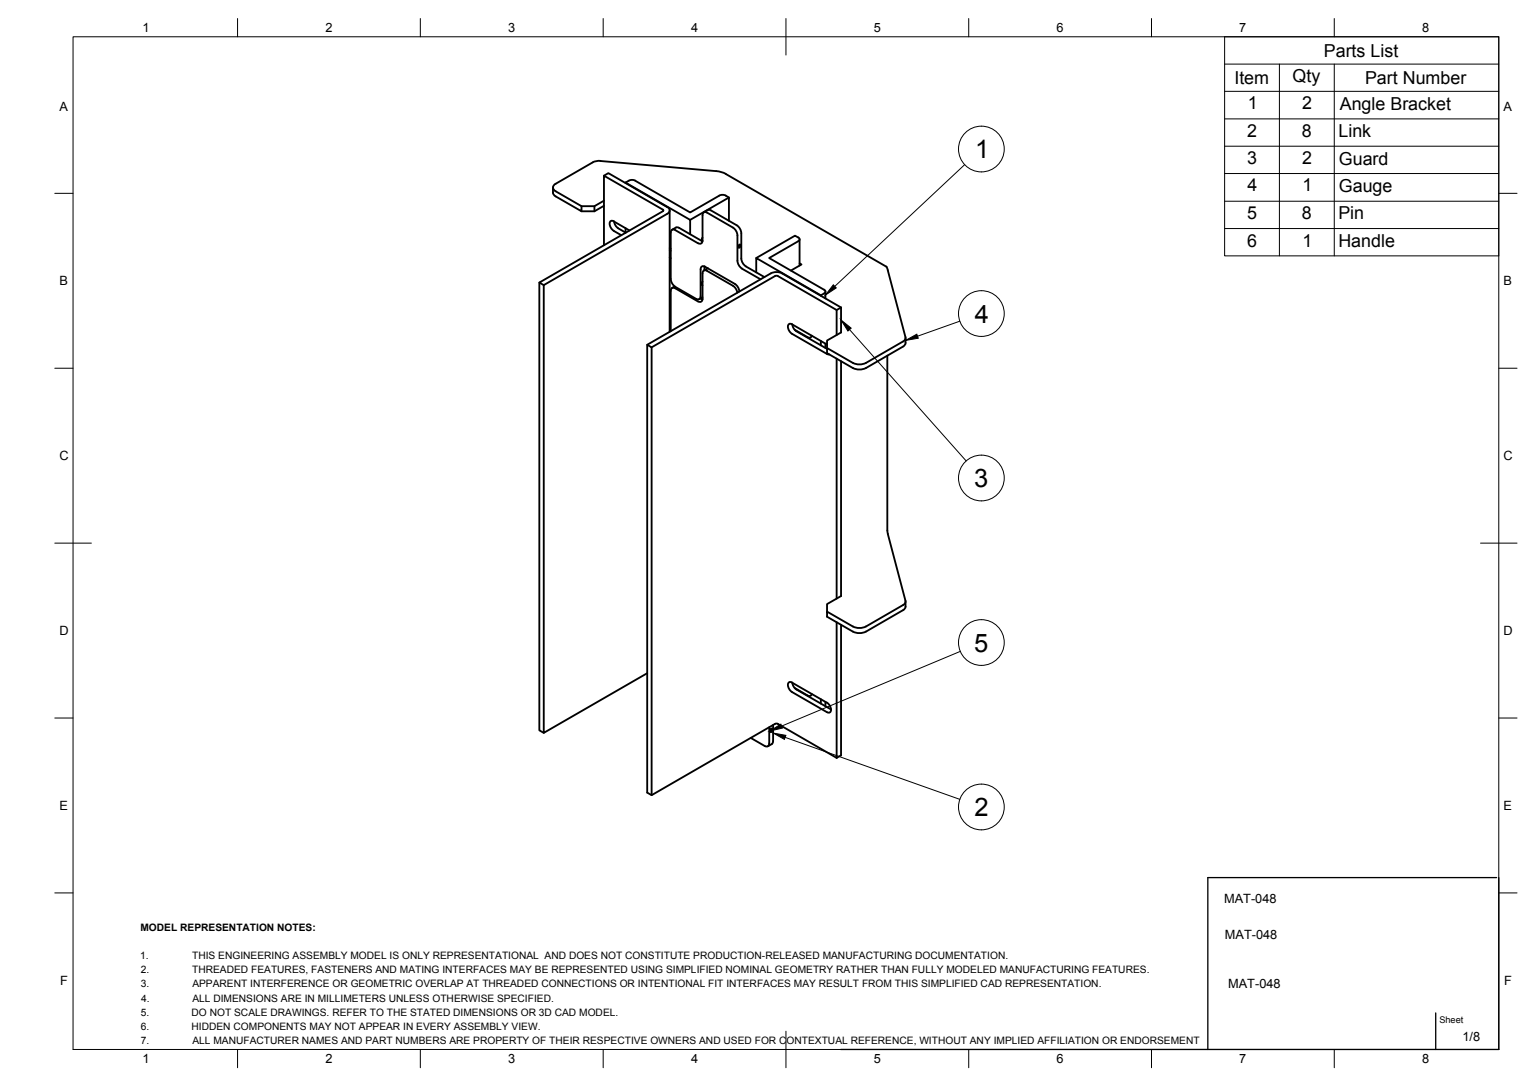
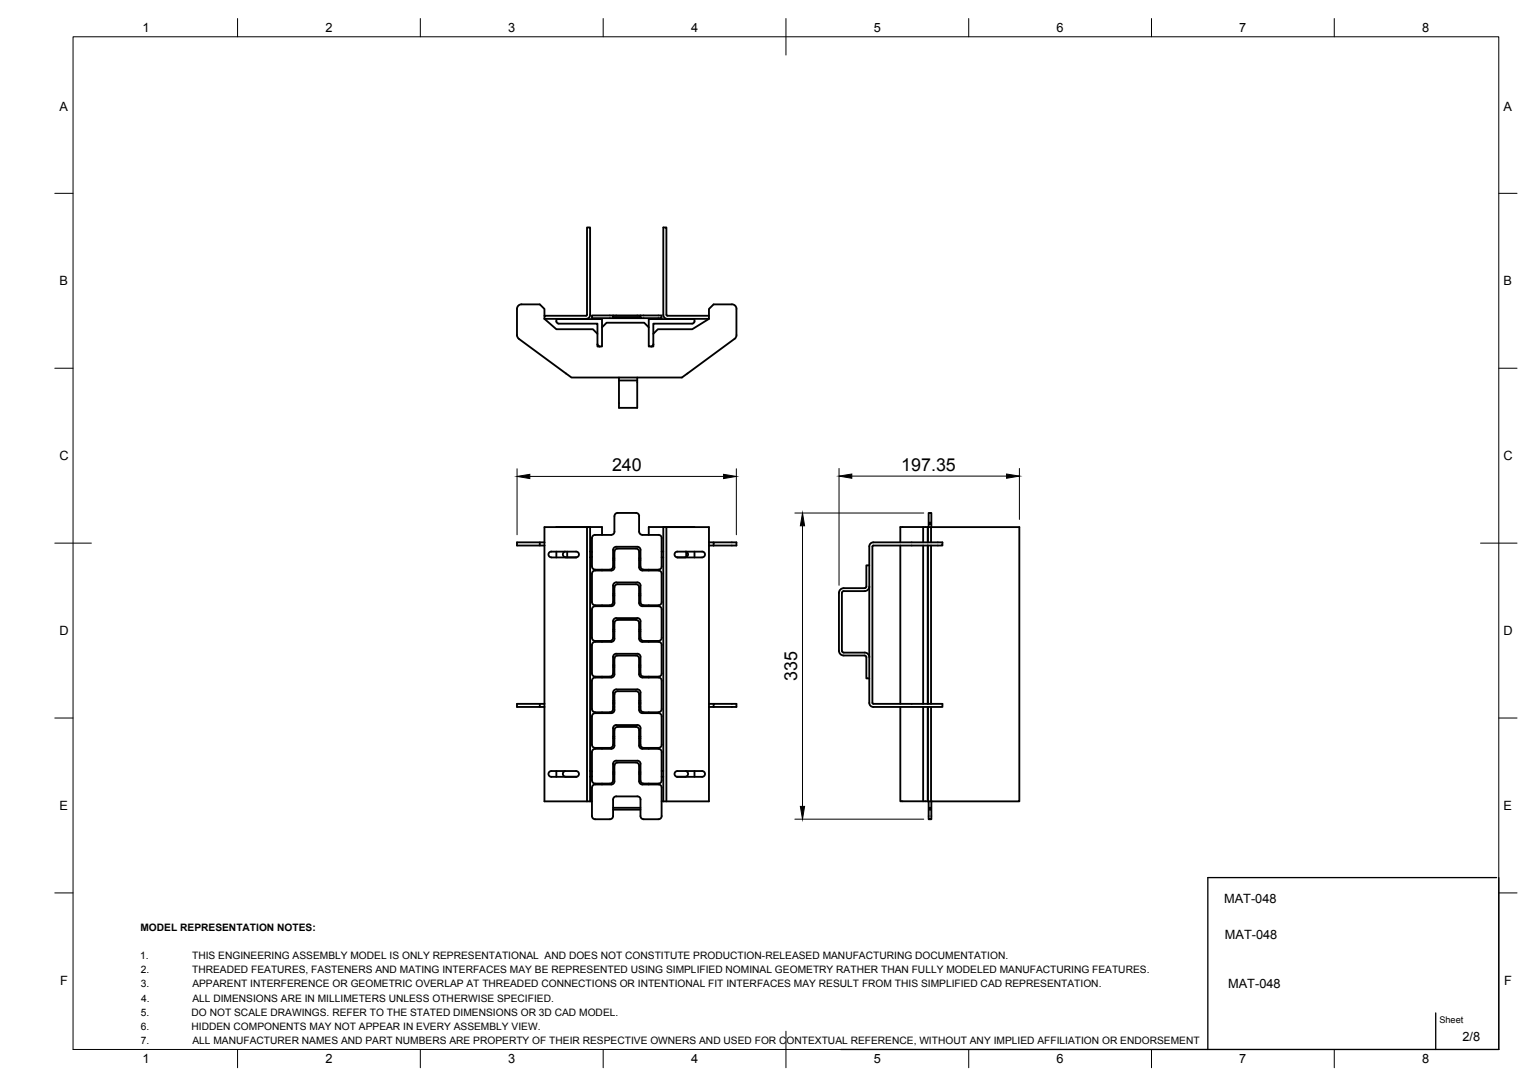
ISO-10303-21;
HEADER;
/* Generated by software containing ST-Developer
 * from STEP Tools, Inc. (www.steptools.com) 
 */

FILE_DESCRIPTION(
/* description */ ('STEP AP214'),
/* implementation_level */ '2;1');

FILE_NAME(
/* name */ 'MAT-048.step',
/* time_stamp */ '2026-11-14T22:24:45-08:00',
/* author */ (''),
/* organization */ (''),
/* preprocessor_version */ 'ST-DEVELOPER v20.2',
/* originating_system */ 'Autodesk Translation Framework v15.17.0.0',
/* authorisation */ '');

FILE_SCHEMA (('AUTOMOTIVE_DESIGN { 1 0 10303 214 3 1 1 }'));
ENDSEC;

DATA;
#10=MECHANICAL_DESIGN_GEOMETRIC_PRESENTATION_REPRESENTATION('',(#125,#126,
#127,#128,#129,#130),#5599);
#11=ITEM_DEFINED_TRANSFORMATION($,$,#3527,#3659);
#12=ITEM_DEFINED_TRANSFORMATION($,$,#3593,#3660);
#13=ITEM_DEFINED_TRANSFORMATION($,$,#3558,#3661);
#14=ITEM_DEFINED_TRANSFORMATION($,$,#3381,#3662);
#15=ITEM_DEFINED_TRANSFORMATION($,$,#3653,#3663);
#16=ITEM_DEFINED_TRANSFORMATION($,$,#3472,#3664);
#17=ITEM_DEFINED_TRANSFORMATION($,$,#3527,#3665);
#18=ITEM_DEFINED_TRANSFORMATION($,$,#3593,#3666);
#19=ITEM_DEFINED_TRANSFORMATION($,$,#3593,#3667);
#20=ITEM_DEFINED_TRANSFORMATION($,$,#3593,#3668);
#21=ITEM_DEFINED_TRANSFORMATION($,$,#3558,#3669);
#22=ITEM_DEFINED_TRANSFORMATION($,$,#3593,#3670);
#23=ITEM_DEFINED_TRANSFORMATION($,$,#3593,#3671);
#24=ITEM_DEFINED_TRANSFORMATION($,$,#3593,#3672);
#25=ITEM_DEFINED_TRANSFORMATION($,$,#3593,#3673);
#26=ITEM_DEFINED_TRANSFORMATION($,$,#3653,#3674);
#27=ITEM_DEFINED_TRANSFORMATION($,$,#3653,#3675);
#28=ITEM_DEFINED_TRANSFORMATION($,$,#3653,#3676);
#29=ITEM_DEFINED_TRANSFORMATION($,$,#3653,#3677);
#30=ITEM_DEFINED_TRANSFORMATION($,$,#3653,#3678);
#31=ITEM_DEFINED_TRANSFORMATION($,$,#3653,#3679);
#32=ITEM_DEFINED_TRANSFORMATION($,$,#3653,#3680);
#33=(
REPRESENTATION_RELATIONSHIP($,$,#5643,#5640)
REPRESENTATION_RELATIONSHIP_WITH_TRANSFORMATION(#11)
SHAPE_REPRESENTATION_RELATIONSHIP()
);
#34=(
REPRESENTATION_RELATIONSHIP($,$,#5645,#5640)
REPRESENTATION_RELATIONSHIP_WITH_TRANSFORMATION(#12)
SHAPE_REPRESENTATION_RELATIONSHIP()
);
#35=(
REPRESENTATION_RELATIONSHIP($,$,#5644,#5640)
REPRESENTATION_RELATIONSHIP_WITH_TRANSFORMATION(#13)
SHAPE_REPRESENTATION_RELATIONSHIP()
);
#36=(
REPRESENTATION_RELATIONSHIP($,$,#5641,#5640)
REPRESENTATION_RELATIONSHIP_WITH_TRANSFORMATION(#14)
SHAPE_REPRESENTATION_RELATIONSHIP()
);
#37=(
REPRESENTATION_RELATIONSHIP($,$,#5646,#5640)
REPRESENTATION_RELATIONSHIP_WITH_TRANSFORMATION(#15)
SHAPE_REPRESENTATION_RELATIONSHIP()
);
#38=(
REPRESENTATION_RELATIONSHIP($,$,#5642,#5640)
REPRESENTATION_RELATIONSHIP_WITH_TRANSFORMATION(#16)
SHAPE_REPRESENTATION_RELATIONSHIP()
);
#39=(
REPRESENTATION_RELATIONSHIP($,$,#5643,#5640)
REPRESENTATION_RELATIONSHIP_WITH_TRANSFORMATION(#17)
SHAPE_REPRESENTATION_RELATIONSHIP()
);
#40=(
REPRESENTATION_RELATIONSHIP($,$,#5645,#5640)
REPRESENTATION_RELATIONSHIP_WITH_TRANSFORMATION(#18)
SHAPE_REPRESENTATION_RELATIONSHIP()
);
#41=(
REPRESENTATION_RELATIONSHIP($,$,#5645,#5640)
REPRESENTATION_RELATIONSHIP_WITH_TRANSFORMATION(#19)
SHAPE_REPRESENTATION_RELATIONSHIP()
);
#42=(
REPRESENTATION_RELATIONSHIP($,$,#5645,#5640)
REPRESENTATION_RELATIONSHIP_WITH_TRANSFORMATION(#20)
SHAPE_REPRESENTATION_RELATIONSHIP()
);
#43=(
REPRESENTATION_RELATIONSHIP($,$,#5644,#5640)
REPRESENTATION_RELATIONSHIP_WITH_TRANSFORMATION(#21)
SHAPE_REPRESENTATION_RELATIONSHIP()
);
#44=(
REPRESENTATION_RELATIONSHIP($,$,#5645,#5640)
REPRESENTATION_RELATIONSHIP_WITH_TRANSFORMATION(#22)
SHAPE_REPRESENTATION_RELATIONSHIP()
);
#45=(
REPRESENTATION_RELATIONSHIP($,$,#5645,#5640)
REPRESENTATION_RELATIONSHIP_WITH_TRANSFORMATION(#23)
SHAPE_REPRESENTATION_RELATIONSHIP()
);
#46=(
REPRESENTATION_RELATIONSHIP($,$,#5645,#5640)
REPRESENTATION_RELATIONSHIP_WITH_TRANSFORMATION(#24)
SHAPE_REPRESENTATION_RELATIONSHIP()
);
#47=(
REPRESENTATION_RELATIONSHIP($,$,#5645,#5640)
REPRESENTATION_RELATIONSHIP_WITH_TRANSFORMATION(#25)
SHAPE_REPRESENTATION_RELATIONSHIP()
);
#48=(
REPRESENTATION_RELATIONSHIP($,$,#5646,#5640)
REPRESENTATION_RELATIONSHIP_WITH_TRANSFORMATION(#26)
SHAPE_REPRESENTATION_RELATIONSHIP()
);
#49=(
REPRESENTATION_RELATIONSHIP($,$,#5646,#5640)
REPRESENTATION_RELATIONSHIP_WITH_TRANSFORMATION(#27)
SHAPE_REPRESENTATION_RELATIONSHIP()
);
#50=(
REPRESENTATION_RELATIONSHIP($,$,#5646,#5640)
REPRESENTATION_RELATIONSHIP_WITH_TRANSFORMATION(#28)
SHAPE_REPRESENTATION_RELATIONSHIP()
);
#51=(
REPRESENTATION_RELATIONSHIP($,$,#5646,#5640)
REPRESENTATION_RELATIONSHIP_WITH_TRANSFORMATION(#29)
SHAPE_REPRESENTATION_RELATIONSHIP()
);
#52=(
REPRESENTATION_RELATIONSHIP($,$,#5646,#5640)
REPRESENTATION_RELATIONSHIP_WITH_TRANSFORMATION(#30)
SHAPE_REPRESENTATION_RELATIONSHIP()
);
#53=(
REPRESENTATION_RELATIONSHIP($,$,#5646,#5640)
REPRESENTATION_RELATIONSHIP_WITH_TRANSFORMATION(#31)
SHAPE_REPRESENTATION_RELATIONSHIP()
);
#54=(
REPRESENTATION_RELATIONSHIP($,$,#5646,#5640)
REPRESENTATION_RELATIONSHIP_WITH_TRANSFORMATION(#32)
SHAPE_REPRESENTATION_RELATIONSHIP()
);
#55=CONTEXT_DEPENDENT_SHAPE_REPRESENTATION(#33,#5618);
#56=CONTEXT_DEPENDENT_SHAPE_REPRESENTATION(#34,#5619);
#57=CONTEXT_DEPENDENT_SHAPE_REPRESENTATION(#35,#5620);
#58=CONTEXT_DEPENDENT_SHAPE_REPRESENTATION(#36,#5621);
#59=CONTEXT_DEPENDENT_SHAPE_REPRESENTATION(#37,#5622);
#60=CONTEXT_DEPENDENT_SHAPE_REPRESENTATION(#38,#5623);
#61=CONTEXT_DEPENDENT_SHAPE_REPRESENTATION(#39,#5624);
#62=CONTEXT_DEPENDENT_SHAPE_REPRESENTATION(#40,#5625);
#63=CONTEXT_DEPENDENT_SHAPE_REPRESENTATION(#41,#5626);
#64=CONTEXT_DEPENDENT_SHAPE_REPRESENTATION(#42,#5627);
#65=CONTEXT_DEPENDENT_SHAPE_REPRESENTATION(#43,#5628);
#66=CONTEXT_DEPENDENT_SHAPE_REPRESENTATION(#44,#5629);
#67=CONTEXT_DEPENDENT_SHAPE_REPRESENTATION(#45,#5630);
#68=CONTEXT_DEPENDENT_SHAPE_REPRESENTATION(#46,#5631);
#69=CONTEXT_DEPENDENT_SHAPE_REPRESENTATION(#47,#5632);
#70=CONTEXT_DEPENDENT_SHAPE_REPRESENTATION(#48,#5633);
#71=CONTEXT_DEPENDENT_SHAPE_REPRESENTATION(#49,#5634);
#72=CONTEXT_DEPENDENT_SHAPE_REPRESENTATION(#50,#5635);
#73=CONTEXT_DEPENDENT_SHAPE_REPRESENTATION(#51,#5636);
#74=CONTEXT_DEPENDENT_SHAPE_REPRESENTATION(#52,#5637);
#75=CONTEXT_DEPENDENT_SHAPE_REPRESENTATION(#53,#5638);
#76=CONTEXT_DEPENDENT_SHAPE_REPRESENTATION(#54,#5639);
#77=NEXT_ASSEMBLY_USAGE_OCCURRENCE('Angle Bracket:1','Angle Bracket:1',
'Angle Bracket:1',#5648,#5651,'Angle Bracket:1');
#78=NEXT_ASSEMBLY_USAGE_OCCURRENCE('Link:1','Link:1','Link:1',#5648,#5653,
'Link:1');
#79=NEXT_ASSEMBLY_USAGE_OCCURRENCE('Guard:1','Guard:1','Guard:1',#5648,
#5652,'Guard:1');
#80=NEXT_ASSEMBLY_USAGE_OCCURRENCE('Gauge:1','Gauge:1','Gauge:1',#5648,
#5649,'Gauge:1');
#81=NEXT_ASSEMBLY_USAGE_OCCURRENCE('Pin:1','Pin:1','Pin:1',#5648,#5654,
'Pin:1');
#82=NEXT_ASSEMBLY_USAGE_OCCURRENCE('Handle:1','Handle:1','Handle:1',#5648,
#5650,'Handle:1');
#83=NEXT_ASSEMBLY_USAGE_OCCURRENCE('Angle Bracket:2','Angle Bracket:2',
'Angle Bracket:2',#5648,#5651,'Angle Bracket:2');
#84=NEXT_ASSEMBLY_USAGE_OCCURRENCE('Link:2','Link:2','Link:2',#5648,#5653,
'Link:2');
#85=NEXT_ASSEMBLY_USAGE_OCCURRENCE('Link:3','Link:3','Link:3',#5648,#5653,
'Link:3');
#86=NEXT_ASSEMBLY_USAGE_OCCURRENCE('Link:4','Link:4','Link:4',#5648,#5653,
'Link:4');
#87=NEXT_ASSEMBLY_USAGE_OCCURRENCE('Guard:2','Guard:2','Guard:2',#5648,
#5652,'Guard:2');
#88=NEXT_ASSEMBLY_USAGE_OCCURRENCE('Link:5','Link:5','Link:5',#5648,#5653,
'Link:5');
#89=NEXT_ASSEMBLY_USAGE_OCCURRENCE('Link:6','Link:6','Link:6',#5648,#5653,
'Link:6');
#90=NEXT_ASSEMBLY_USAGE_OCCURRENCE('Link:7','Link:7','Link:7',#5648,#5653,
'Link:7');
#91=NEXT_ASSEMBLY_USAGE_OCCURRENCE('Link:8','Link:8','Link:8',#5648,#5653,
'Link:8');
#92=NEXT_ASSEMBLY_USAGE_OCCURRENCE('Pin:2','Pin:2','Pin:2',#5648,#5654,
'Pin:2');
#93=NEXT_ASSEMBLY_USAGE_OCCURRENCE('Pin:3','Pin:3','Pin:3',#5648,#5654,
'Pin:3');
#94=NEXT_ASSEMBLY_USAGE_OCCURRENCE('Pin:4','Pin:4','Pin:4',#5648,#5654,
'Pin:4');
#95=NEXT_ASSEMBLY_USAGE_OCCURRENCE('Pin:5','Pin:5','Pin:5',#5648,#5654,
'Pin:5');
#96=NEXT_ASSEMBLY_USAGE_OCCURRENCE('Pin:6','Pin:6','Pin:6',#5648,#5654,
'Pin:6');
#97=NEXT_ASSEMBLY_USAGE_OCCURRENCE('Pin:7','Pin:7','Pin:7',#5648,#5654,
'Pin:7');
#98=NEXT_ASSEMBLY_USAGE_OCCURRENCE('Pin:8','Pin:8','Pin:8',#5648,#5654,
'Pin:8');
#99=FACE_BOUND('',#563,.T.);
#100=FACE_BOUND('',#564,.T.);
#101=FACE_BOUND('',#570,.T.);
#102=FACE_BOUND('',#571,.T.);
#103=FACE_BOUND('',#588,.T.);
#104=FACE_BOUND('',#589,.T.);
#105=FACE_BOUND('',#592,.T.);
#106=FACE_BOUND('',#593,.T.);
#107=FACE_BOUND('',#614,.T.);
#108=FACE_BOUND('',#619,.T.);
#109=FACE_BOUND('',#624,.T.);
#110=FACE_BOUND('',#629,.T.);
#111=FACE_BOUND('',#634,.T.);
#112=FACE_BOUND('',#639,.T.);
#113=SHAPE_REPRESENTATION_RELATIONSHIP('SRR','None',#5641,#119);
#114=SHAPE_REPRESENTATION_RELATIONSHIP('SRR','None',#5642,#120);
#115=SHAPE_REPRESENTATION_RELATIONSHIP('SRR','None',#5643,#121);
#116=SHAPE_REPRESENTATION_RELATIONSHIP('SRR','None',#5644,#122);
#117=SHAPE_REPRESENTATION_RELATIONSHIP('SRR','None',#5645,#123);
#118=SHAPE_REPRESENTATION_RELATIONSHIP('SRR','None',#5646,#124);
#119=ADVANCED_BREP_SHAPE_REPRESENTATION('',(#131),#5593);
#120=ADVANCED_BREP_SHAPE_REPRESENTATION('',(#132),#5594);
#121=ADVANCED_BREP_SHAPE_REPRESENTATION('',(#133),#5595);
#122=ADVANCED_BREP_SHAPE_REPRESENTATION('',(#134),#5596);
#123=ADVANCED_BREP_SHAPE_REPRESENTATION('',(#135),#5597);
#124=ADVANCED_BREP_SHAPE_REPRESENTATION('',(#136),#5598);
#125=STYLED_ITEM('',(#5680),#131);
#126=STYLED_ITEM('',(#5681),#132);
#127=STYLED_ITEM('',(#5681),#133);
#128=STYLED_ITEM('',(#5680),#134);
#129=STYLED_ITEM('',(#5680),#135);
#130=STYLED_ITEM('',(#5680),#136);
#131=MANIFOLD_SOLID_BREP('Body1',#3307);
#132=MANIFOLD_SOLID_BREP('Body1',#3308);
#133=MANIFOLD_SOLID_BREP('Body1',#3309);
#134=MANIFOLD_SOLID_BREP('Body1',#3310);
#135=MANIFOLD_SOLID_BREP('Body1',#3311);
#136=MANIFOLD_SOLID_BREP('Body1',#3312);
#137=ELLIPSE('',#3398,7.45592114551632,4.41999999999987);
#138=ELLIPSE('',#3399,7.45592114551703,4.42000000000052);
#139=ELLIPSE('',#3402,7.45592114551723,4.42000000000049);
#140=ELLIPSE('',#3403,7.45592114551628,4.41999999999988);
#141=ELLIPSE('',#3416,1.68685998767419,1.00000000000061);
#142=ELLIPSE('',#3417,1.68685998767298,0.999999999999771);
#143=ELLIPSE('',#3420,1.68685998767017,0.999999999998458);
#144=ELLIPSE('',#3421,1.68685998767381,1.0000000000002);
#145=CYLINDRICAL_SURFACE('',#3397,4.42000000000001);
#146=CYLINDRICAL_SURFACE('',#3401,4.42);
#147=CYLINDRICAL_SURFACE('',#3415,1.);
#148=CYLINDRICAL_SURFACE('',#3419,1.);
#149=CYLINDRICAL_SURFACE('',#3464,5.);
#150=CYLINDRICAL_SURFACE('',#3465,5.);
#151=CYLINDRICAL_SURFACE('',#3466,5.);
#152=CYLINDRICAL_SURFACE('',#3467,5.);
#153=CYLINDRICAL_SURFACE('',#3468,5.);
#154=CYLINDRICAL_SURFACE('',#3469,5.);
#155=CYLINDRICAL_SURFACE('',#3470,5.);
#156=CYLINDRICAL_SURFACE('',#3471,5.);
#157=CYLINDRICAL_SURFACE('',#3508,2.);
#158=CYLINDRICAL_SURFACE('',#3510,5.175);
#159=CYLINDRICAL_SURFACE('',#3512,5.175);
#160=CYLINDRICAL_SURFACE('',#3514,2.);
#161=CYLINDRICAL_SURFACE('',#3518,5.175);
#162=CYLINDRICAL_SURFACE('',#3520,2.);
#163=CYLINDRICAL_SURFACE('',#3522,2.);
#164=CYLINDRICAL_SURFACE('',#3524,5.175);
#165=CYLINDRICAL_SURFACE('',#3536,2.5);
#166=CYLINDRICAL_SURFACE('',#3545,2.5);
#167=CYLINDRICAL_SURFACE('',#3550,3.17499999999993);
#168=CYLINDRICAL_SURFACE('',#3552,3.17499999999993);
#169=CYLINDRICAL_SURFACE('',#3554,3.17499999999993);
#170=CYLINDRICAL_SURFACE('',#3556,3.17499999999993);
#171=CYLINDRICAL_SURFACE('',#3578,4.42);
#172=CYLINDRICAL_SURFACE('',#3582,1.);
#173=CYLINDRICAL_SURFACE('',#3585,3.17500000000003);
#174=CYLINDRICAL_SURFACE('',#3587,3.17500000000002);
#175=CYLINDRICAL_SURFACE('',#3589,3.17500000000004);
#176=CYLINDRICAL_SURFACE('',#3591,3.17500000000004);
#177=CYLINDRICAL_SURFACE('',#3594,0.999999999999991);
#178=CYLINDRICAL_SURFACE('',#3597,0.999999999999991);
#179=CYLINDRICAL_SURFACE('',#3600,1.);
#180=CYLINDRICAL_SURFACE('',#3603,3.5);
#181=CYLINDRICAL_SURFACE('',#3607,3.5);
#182=CYLINDRICAL_SURFACE('',#3611,3.5);
#183=CYLINDRICAL_SURFACE('',#3615,3.5);
#184=CYLINDRICAL_SURFACE('',#3619,3.5);
#185=CYLINDRICAL_SURFACE('',#3623,3.5);
#186=CYLINDRICAL_SURFACE('',#3627,3.5);
#187=CYLINDRICAL_SURFACE('',#3631,3.5);
#188=CYLINDRICAL_SURFACE('',#3635,3.5);
#189=CYLINDRICAL_SURFACE('',#3639,3.5);
#190=CYLINDRICAL_SURFACE('',#3643,3.5);
#191=CYLINDRICAL_SURFACE('',#3647,3.5);
#192=CYLINDRICAL_SURFACE('',#3654,1.);
#193=CIRCLE('',#3387,5.);
#194=CIRCLE('',#3388,5.);
#195=CIRCLE('',#3389,5.);
#196=CIRCLE('',#3390,5.);
#197=CIRCLE('',#3393,5.);
#198=CIRCLE('',#3394,5.);
#199=CIRCLE('',#3395,5.);
#200=CIRCLE('',#3396,5.);
#201=CIRCLE('',#3405,5.);
#202=CIRCLE('',#3406,5.);
#203=CIRCLE('',#3407,5.);
#204=CIRCLE('',#3408,5.);
#205=CIRCLE('',#3411,5.);
#206=CIRCLE('',#3412,5.);
#207=CIRCLE('',#3413,5.);
#208=CIRCLE('',#3414,5.);
#209=CIRCLE('',#3474,2.);
#210=CIRCLE('',#3475,5.175);
#211=CIRCLE('',#3478,2.);
#212=CIRCLE('',#3479,5.175);
#213=CIRCLE('',#3482,5.175);
#214=CIRCLE('',#3483,2.);
#215=CIRCLE('',#3486,5.175);
#216=CIRCLE('',#3487,2.);
#217=CIRCLE('',#3490,5.175);
#218=CIRCLE('',#3491,2.);
#219=CIRCLE('',#3494,5.175);
#220=CIRCLE('',#3495,2.);
#221=CIRCLE('',#3498,2.);
#222=CIRCLE('',#3499,5.175);
#223=CIRCLE('',#3502,2.);
#224=CIRCLE('',#3503,5.175);
#225=CIRCLE('',#3530,3.17499999999993);
#226=CIRCLE('',#3531,3.17499999999993);
#227=CIRCLE('',#3532,3.17499999999993);
#228=CIRCLE('',#3533,3.17499999999993);
#229=CIRCLE('',#3537,2.5);
#230=CIRCLE('',#3538,2.5);
#231=CIRCLE('',#3541,3.17499999999993);
#232=CIRCLE('',#3542,3.17499999999993);
#233=CIRCLE('',#3543,3.17499999999993);
#234=CIRCLE('',#3544,3.17499999999993);
#235=CIRCLE('',#3546,2.5);
#236=CIRCLE('',#3547,2.5);
#237=CIRCLE('',#3560,4.42);
#238=CIRCLE('',#3561,1.);
#239=CIRCLE('',#3564,4.42);
#240=CIRCLE('',#3565,1.);
#241=CIRCLE('',#3568,3.17500000000004);
#242=CIRCLE('',#3569,3.17500000000004);
#243=CIRCLE('',#3570,3.17500000000003);
#244=CIRCLE('',#3571,3.17500000000002);
#245=CIRCLE('',#3574,3.17500000000004);
#246=CIRCLE('',#3575,3.17500000000004);
#247=CIRCLE('',#3576,3.17500000000003);
#248=CIRCLE('',#3577,3.17500000000002);
#249=CIRCLE('',#3595,0.999999999999991);
#250=CIRCLE('',#3596,0.999999999999991);
#251=CIRCLE('',#3598,0.999999999999991);
#252=CIRCLE('',#3599,0.999999999999991);
#253=CIRCLE('',#3601,0.999999999999988);
#254=CIRCLE('',#3602,1.);
#255=CIRCLE('',#3604,3.5);
#256=CIRCLE('',#3605,3.5);
#257=CIRCLE('',#3608,3.5);
#258=CIRCLE('',#3609,3.5);
#259=CIRCLE('',#3612,3.5);
#260=CIRCLE('',#3613,3.5);
#261=CIRCLE('',#3616,3.5);
#262=CIRCLE('',#3617,3.5);
#263=CIRCLE('',#3620,3.5);
#264=CIRCLE('',#3621,3.5);
#265=CIRCLE('',#3624,3.5);
#266=CIRCLE('',#3625,3.5);
#267=CIRCLE('',#3628,3.5);
#268=CIRCLE('',#3629,3.5);
#269=CIRCLE('',#3632,3.5);
#270=CIRCLE('',#3633,3.5);
#271=CIRCLE('',#3636,3.5);
#272=CIRCLE('',#3637,3.5);
#273=CIRCLE('',#3640,3.5);
#274=CIRCLE('',#3641,3.5);
#275=CIRCLE('',#3644,3.5);
#276=CIRCLE('',#3645,3.5);
#277=CIRCLE('',#3648,3.5);
#278=CIRCLE('',#3649,3.5);
#279=CIRCLE('',#3655,1.);
#280=CIRCLE('',#3656,1.);
#281=FACE_OUTER_BOUND('',#457,.T.);
#282=FACE_OUTER_BOUND('',#458,.T.);
#283=FACE_OUTER_BOUND('',#459,.T.);
#284=FACE_OUTER_BOUND('',#460,.T.);
#285=FACE_OUTER_BOUND('',#461,.T.);
#286=FACE_OUTER_BOUND('',#462,.T.);
#287=FACE_OUTER_BOUND('',#463,.T.);
#288=FACE_OUTER_BOUND('',#464,.T.);
#289=FACE_OUTER_BOUND('',#465,.T.);
#290=FACE_OUTER_BOUND('',#466,.T.);
#291=FACE_OUTER_BOUND('',#467,.T.);
#292=FACE_OUTER_BOUND('',#468,.T.);
#293=FACE_OUTER_BOUND('',#469,.T.);
#294=FACE_OUTER_BOUND('',#470,.T.);
#295=FACE_OUTER_BOUND('',#471,.T.);
#296=FACE_OUTER_BOUND('',#472,.T.);
#297=FACE_OUTER_BOUND('',#473,.T.);
#298=FACE_OUTER_BOUND('',#474,.T.);
#299=FACE_OUTER_BOUND('',#475,.T.);
#300=FACE_OUTER_BOUND('',#476,.T.);
#301=FACE_OUTER_BOUND('',#477,.T.);
#302=FACE_OUTER_BOUND('',#478,.T.);
#303=FACE_OUTER_BOUND('',#479,.T.);
#304=FACE_OUTER_BOUND('',#480,.T.);
#305=FACE_OUTER_BOUND('',#481,.T.);
#306=FACE_OUTER_BOUND('',#482,.T.);
#307=FACE_OUTER_BOUND('',#483,.T.);
#308=FACE_OUTER_BOUND('',#484,.T.);
#309=FACE_OUTER_BOUND('',#485,.T.);
#310=FACE_OUTER_BOUND('',#486,.T.);
#311=FACE_OUTER_BOUND('',#487,.T.);
#312=FACE_OUTER_BOUND('',#488,.T.);
#313=FACE_OUTER_BOUND('',#489,.T.);
#314=FACE_OUTER_BOUND('',#490,.T.);
#315=FACE_OUTER_BOUND('',#491,.T.);
#316=FACE_OUTER_BOUND('',#492,.T.);
#317=FACE_OUTER_BOUND('',#493,.T.);
#318=FACE_OUTER_BOUND('',#494,.T.);
#319=FACE_OUTER_BOUND('',#495,.T.);
#320=FACE_OUTER_BOUND('',#496,.T.);
#321=FACE_OUTER_BOUND('',#497,.T.);
#322=FACE_OUTER_BOUND('',#498,.T.);
#323=FACE_OUTER_BOUND('',#499,.T.);
#324=FACE_OUTER_BOUND('',#500,.T.);
#325=FACE_OUTER_BOUND('',#501,.T.);
#326=FACE_OUTER_BOUND('',#502,.T.);
#327=FACE_OUTER_BOUND('',#503,.T.);
#328=FACE_OUTER_BOUND('',#504,.T.);
#329=FACE_OUTER_BOUND('',#505,.T.);
#330=FACE_OUTER_BOUND('',#506,.T.);
#331=FACE_OUTER_BOUND('',#507,.T.);
#332=FACE_OUTER_BOUND('',#508,.T.);
#333=FACE_OUTER_BOUND('',#509,.T.);
#334=FACE_OUTER_BOUND('',#510,.T.);
#335=FACE_OUTER_BOUND('',#511,.T.);
#336=FACE_OUTER_BOUND('',#512,.T.);
#337=FACE_OUTER_BOUND('',#513,.T.);
#338=FACE_OUTER_BOUND('',#514,.T.);
#339=FACE_OUTER_BOUND('',#515,.T.);
#340=FACE_OUTER_BOUND('',#516,.T.);
#341=FACE_OUTER_BOUND('',#517,.T.);
#342=FACE_OUTER_BOUND('',#518,.T.);
#343=FACE_OUTER_BOUND('',#519,.T.);
#344=FACE_OUTER_BOUND('',#520,.T.);
#345=FACE_OUTER_BOUND('',#521,.T.);
#346=FACE_OUTER_BOUND('',#522,.T.);
#347=FACE_OUTER_BOUND('',#523,.T.);
#348=FACE_OUTER_BOUND('',#524,.T.);
#349=FACE_OUTER_BOUND('',#525,.T.);
#350=FACE_OUTER_BOUND('',#526,.T.);
#351=FACE_OUTER_BOUND('',#527,.T.);
#352=FACE_OUTER_BOUND('',#528,.T.);
#353=FACE_OUTER_BOUND('',#529,.T.);
#354=FACE_OUTER_BOUND('',#530,.T.);
#355=FACE_OUTER_BOUND('',#531,.T.);
#356=FACE_OUTER_BOUND('',#532,.T.);
#357=FACE_OUTER_BOUND('',#533,.T.);
#358=FACE_OUTER_BOUND('',#534,.T.);
#359=FACE_OUTER_BOUND('',#535,.T.);
#360=FACE_OUTER_BOUND('',#536,.T.);
#361=FACE_OUTER_BOUND('',#537,.T.);
#362=FACE_OUTER_BOUND('',#538,.T.);
#363=FACE_OUTER_BOUND('',#539,.T.);
#364=FACE_OUTER_BOUND('',#540,.T.);
#365=FACE_OUTER_BOUND('',#541,.T.);
#366=FACE_OUTER_BOUND('',#542,.T.);
#367=FACE_OUTER_BOUND('',#543,.T.);
#368=FACE_OUTER_BOUND('',#544,.T.);
#369=FACE_OUTER_BOUND('',#545,.T.);
#370=FACE_OUTER_BOUND('',#546,.T.);
#371=FACE_OUTER_BOUND('',#547,.T.);
#372=FACE_OUTER_BOUND('',#548,.T.);
#373=FACE_OUTER_BOUND('',#549,.T.);
#374=FACE_OUTER_BOUND('',#550,.T.);
#375=FACE_OUTER_BOUND('',#551,.T.);
#376=FACE_OUTER_BOUND('',#552,.T.);
#377=FACE_OUTER_BOUND('',#553,.T.);
#378=FACE_OUTER_BOUND('',#554,.T.);
#379=FACE_OUTER_BOUND('',#555,.T.);
#380=FACE_OUTER_BOUND('',#556,.T.);
#381=FACE_OUTER_BOUND('',#557,.T.);
#382=FACE_OUTER_BOUND('',#558,.T.);
#383=FACE_OUTER_BOUND('',#559,.T.);
#384=FACE_OUTER_BOUND('',#560,.T.);
#385=FACE_OUTER_BOUND('',#561,.T.);
#386=FACE_OUTER_BOUND('',#562,.T.);
#387=FACE_OUTER_BOUND('',#565,.T.);
#388=FACE_OUTER_BOUND('',#566,.T.);
#389=FACE_OUTER_BOUND('',#567,.T.);
#390=FACE_OUTER_BOUND('',#568,.T.);
#391=FACE_OUTER_BOUND('',#569,.T.);
#392=FACE_OUTER_BOUND('',#572,.T.);
#393=FACE_OUTER_BOUND('',#573,.T.);
#394=FACE_OUTER_BOUND('',#574,.T.);
#395=FACE_OUTER_BOUND('',#575,.T.);
#396=FACE_OUTER_BOUND('',#576,.T.);
#397=FACE_OUTER_BOUND('',#577,.T.);
#398=FACE_OUTER_BOUND('',#578,.T.);
#399=FACE_OUTER_BOUND('',#579,.T.);
#400=FACE_OUTER_BOUND('',#580,.T.);
#401=FACE_OUTER_BOUND('',#581,.T.);
#402=FACE_OUTER_BOUND('',#582,.T.);
#403=FACE_OUTER_BOUND('',#583,.T.);
#404=FACE_OUTER_BOUND('',#584,.T.);
#405=FACE_OUTER_BOUND('',#585,.T.);
#406=FACE_OUTER_BOUND('',#586,.T.);
#407=FACE_OUTER_BOUND('',#587,.T.);
#408=FACE_OUTER_BOUND('',#590,.T.);
#409=FACE_OUTER_BOUND('',#591,.T.);
#410=FACE_OUTER_BOUND('',#594,.T.);
#411=FACE_OUTER_BOUND('',#595,.T.);
#412=FACE_OUTER_BOUND('',#596,.T.);
#413=FACE_OUTER_BOUND('',#597,.T.);
#414=FACE_OUTER_BOUND('',#598,.T.);
#415=FACE_OUTER_BOUND('',#599,.T.);
#416=FACE_OUTER_BOUND('',#600,.T.);
#417=FACE_OUTER_BOUND('',#601,.T.);
#418=FACE_OUTER_BOUND('',#602,.T.);
#419=FACE_OUTER_BOUND('',#603,.T.);
#420=FACE_OUTER_BOUND('',#604,.T.);
#421=FACE_OUTER_BOUND('',#605,.T.);
#422=FACE_OUTER_BOUND('',#606,.T.);
#423=FACE_OUTER_BOUND('',#607,.T.);
#424=FACE_OUTER_BOUND('',#608,.T.);
#425=FACE_OUTER_BOUND('',#609,.T.);
#426=FACE_OUTER_BOUND('',#610,.T.);
#427=FACE_OUTER_BOUND('',#611,.T.);
#428=FACE_OUTER_BOUND('',#612,.T.);
#429=FACE_OUTER_BOUND('',#613,.T.);
#430=FACE_OUTER_BOUND('',#615,.T.);
#431=FACE_OUTER_BOUND('',#616,.T.);
#432=FACE_OUTER_BOUND('',#617,.T.);
#433=FACE_OUTER_BOUND('',#618,.T.);
#434=FACE_OUTER_BOUND('',#620,.T.);
#435=FACE_OUTER_BOUND('',#621,.T.);
#436=FACE_OUTER_BOUND('',#622,.T.);
#437=FACE_OUTER_BOUND('',#623,.T.);
#438=FACE_OUTER_BOUND('',#625,.T.);
#439=FACE_OUTER_BOUND('',#626,.T.);
#440=FACE_OUTER_BOUND('',#627,.T.);
#441=FACE_OUTER_BOUND('',#628,.T.);
#442=FACE_OUTER_BOUND('',#630,.T.);
#443=FACE_OUTER_BOUND('',#631,.T.);
#444=FACE_OUTER_BOUND('',#632,.T.);
#445=FACE_OUTER_BOUND('',#633,.T.);
#446=FACE_OUTER_BOUND('',#635,.T.);
#447=FACE_OUTER_BOUND('',#636,.T.);
#448=FACE_OUTER_BOUND('',#637,.T.);
#449=FACE_OUTER_BOUND('',#638,.T.);
#450=FACE_OUTER_BOUND('',#640,.T.);
#451=FACE_OUTER_BOUND('',#641,.T.);
#452=FACE_OUTER_BOUND('',#642,.T.);
#453=FACE_OUTER_BOUND('',#643,.T.);
#454=FACE_OUTER_BOUND('',#644,.T.);
#455=FACE_OUTER_BOUND('',#645,.T.);
#456=FACE_OUTER_BOUND('',#646,.T.);
#457=EDGE_LOOP('',(#2099,#2100,#2101,#2102));
#458=EDGE_LOOP('',(#2103,#2104,#2105,#2106));
#459=EDGE_LOOP('',(#2107,#2108,#2109,#2110));
#460=EDGE_LOOP('',(#2111,#2112,#2113,#2114));
#461=EDGE_LOOP('',(#2115,#2116,#2117,#2118,#2119,#2120,#2121,#2122,#2123,
#2124,#2125,#2126,#2127,#2128,#2129,#2130,#2131,#2132,#2133,#2134,#2135,
#2136,#2137,#2138,#2139,#2140,#2141,#2142,#2143,#2144));
#462=EDGE_LOOP('',(#2145,#2146,#2147,#2148));
#463=EDGE_LOOP('',(#2149,#2150,#2151,#2152,#2153,#2154,#2155,#2156,#2157,
#2158,#2159,#2160,#2161,#2162,#2163,#2164,#2165,#2166,#2167,#2168,#2169,
#2170,#2171,#2172,#2173,#2174,#2175,#2176,#2177,#2178));
#464=EDGE_LOOP('',(#2179,#2180,#2181,#2182));
#465=EDGE_LOOP('',(#2183,#2184,#2185,#2186));
#466=EDGE_LOOP('',(#2187,#2188,#2189,#2190));
#467=EDGE_LOOP('',(#2191,#2192,#2193,#2194,#2195,#2196,#2197,#2198,#2199,
#2200,#2201,#2202,#2203,#2204,#2205,#2206,#2207,#2208,#2209,#2210,#2211,
#2212,#2213,#2214,#2215,#2216,#2217,#2218,#2219,#2220));
#468=EDGE_LOOP('',(#2221,#2222,#2223,#2224));
#469=EDGE_LOOP('',(#2225,#2226,#2227,#2228,#2229,#2230,#2231,#2232,#2233,
#2234,#2235,#2236,#2237,#2238,#2239,#2240,#2241,#2242,#2243,#2244,#2245,
#2246,#2247,#2248,#2249,#2250,#2251,#2252,#2253,#2254));
#470=EDGE_LOOP('',(#2255,#2256,#2257,#2258));
#471=EDGE_LOOP('',(#2259,#2260,#2261,#2262));
#472=EDGE_LOOP('',(#2263,#2264,#2265,#2266));
#473=EDGE_LOOP('',(#2267,#2268,#2269,#2270));
#474=EDGE_LOOP('',(#2271,#2272,#2273,#2274));
#475=EDGE_LOOP('',(#2275,#2276,#2277,#2278,#2279,#2280,#2281,#2282,#2283,
#2284,#2285,#2286));
#476=EDGE_LOOP('',(#2287,#2288,#2289,#2290,#2291,#2292,#2293,#2294,#2295,
#2296,#2297,#2298));
#477=EDGE_LOOP('',(#2299,#2300,#2301,#2302));
#478=EDGE_LOOP('',(#2303,#2304,#2305,#2306));
#479=EDGE_LOOP('',(#2307,#2308,#2309,#2310));
#480=EDGE_LOOP('',(#2311,#2312,#2313,#2314));
#481=EDGE_LOOP('',(#2315,#2316,#2317,#2318));
#482=EDGE_LOOP('',(#2319,#2320,#2321,#2322));
#483=EDGE_LOOP('',(#2323,#2324,#2325,#2326));
#484=EDGE_LOOP('',(#2327,#2328,#2329,#2330));
#485=EDGE_LOOP('',(#2331,#2332,#2333,#2334));
#486=EDGE_LOOP('',(#2335,#2336,#2337,#2338));
#487=EDGE_LOOP('',(#2339,#2340,#2341,#2342));
#488=EDGE_LOOP('',(#2343,#2344,#2345,#2346));
#489=EDGE_LOOP('',(#2347,#2348,#2349,#2350));
#490=EDGE_LOOP('',(#2351,#2352,#2353,#2354));
#491=EDGE_LOOP('',(#2355,#2356,#2357,#2358));
#492=EDGE_LOOP('',(#2359,#2360,#2361,#2362));
#493=EDGE_LOOP('',(#2363,#2364,#2365,#2366));
#494=EDGE_LOOP('',(#2367,#2368,#2369,#2370));
#495=EDGE_LOOP('',(#2371,#2372,#2373,#2374));
#496=EDGE_LOOP('',(#2375,#2376,#2377,#2378));
#497=EDGE_LOOP('',(#2379,#2380,#2381,#2382));
#498=EDGE_LOOP('',(#2383,#2384,#2385,#2386));
#499=EDGE_LOOP('',(#2387,#2388,#2389,#2390));
#500=EDGE_LOOP('',(#2391,#2392,#2393,#2394));
#501=EDGE_LOOP('',(#2395,#2396,#2397,#2398));
#502=EDGE_LOOP('',(#2399,#2400,#2401,#2402));
#503=EDGE_LOOP('',(#2403,#2404,#2405,#2406));
#504=EDGE_LOOP('',(#2407,#2408,#2409,#2410));
#505=EDGE_LOOP('',(#2411,#2412,#2413,#2414));
#506=EDGE_LOOP('',(#2415,#2416,#2417,#2418));
#507=EDGE_LOOP('',(#2419,#2420,#2421,#2422));
#508=EDGE_LOOP('',(#2423,#2424,#2425,#2426));
#509=EDGE_LOOP('',(#2427,#2428,#2429,#2430));
#510=EDGE_LOOP('',(#2431,#2432,#2433,#2434));
#511=EDGE_LOOP('',(#2435,#2436,#2437,#2438));
#512=EDGE_LOOP('',(#2439,#2440,#2441,#2442));
#513=EDGE_LOOP('',(#2443,#2444,#2445,#2446));
#514=EDGE_LOOP('',(#2447,#2448,#2449,#2450));
#515=EDGE_LOOP('',(#2451,#2452,#2453,#2454));
#516=EDGE_LOOP('',(#2455,#2456,#2457,#2458));
#517=EDGE_LOOP('',(#2459,#2460,#2461,#2462));
#518=EDGE_LOOP('',(#2463,#2464,#2465,#2466));
#519=EDGE_LOOP('',(#2467,#2468,#2469,#2470));
#520=EDGE_LOOP('',(#2471,#2472,#2473,#2474));
#521=EDGE_LOOP('',(#2475,#2476,#2477,#2478));
#522=EDGE_LOOP('',(#2479,#2480,#2481,#2482));
#523=EDGE_LOOP('',(#2483,#2484,#2485,#2486));
#524=EDGE_LOOP('',(#2487,#2488,#2489,#2490));
#525=EDGE_LOOP('',(#2491,#2492,#2493,#2494));
#526=EDGE_LOOP('',(#2495,#2496,#2497,#2498));
#527=EDGE_LOOP('',(#2499,#2500,#2501,#2502));
#528=EDGE_LOOP('',(#2503,#2504,#2505,#2506));
#529=EDGE_LOOP('',(#2507,#2508,#2509,#2510));
#530=EDGE_LOOP('',(#2511,#2512,#2513,#2514));
#531=EDGE_LOOP('',(#2515,#2516,#2517,#2518));
#532=EDGE_LOOP('',(#2519,#2520,#2521,#2522));
#533=EDGE_LOOP('',(#2523,#2524,#2525,#2526));
#534=EDGE_LOOP('',(#2527,#2528,#2529,#2530));
#535=EDGE_LOOP('',(#2531,#2532,#2533,#2534));
#536=EDGE_LOOP('',(#2535,#2536,#2537,#2538));
#537=EDGE_LOOP('',(#2539,#2540,#2541,#2542));
#538=EDGE_LOOP('',(#2543,#2544,#2545,#2546));
#539=EDGE_LOOP('',(#2547,#2548,#2549,#2550));
#540=EDGE_LOOP('',(#2551,#2552,#2553,#2554));
#541=EDGE_LOOP('',(#2555,#2556,#2557,#2558));
#542=EDGE_LOOP('',(#2559,#2560,#2561,#2562));
#543=EDGE_LOOP('',(#2563,#2564,#2565,#2566));
#544=EDGE_LOOP('',(#2567,#2568,#2569,#2570));
#545=EDGE_LOOP('',(#2571,#2572,#2573,#2574));
#546=EDGE_LOOP('',(#2575,#2576,#2577,#2578));
#547=EDGE_LOOP('',(#2579,#2580,#2581,#2582));
#548=EDGE_LOOP('',(#2583,#2584,#2585,#2586));
#549=EDGE_LOOP('',(#2587,#2588,#2589,#2590));
#550=EDGE_LOOP('',(#2591,#2592,#2593,#2594));
#551=EDGE_LOOP('',(#2595,#2596,#2597,#2598));
#552=EDGE_LOOP('',(#2599,#2600,#2601,#2602));
#553=EDGE_LOOP('',(#2603,#2604,#2605,#2606));
#554=EDGE_LOOP('',(#2607,#2608,#2609,#2610));
#555=EDGE_LOOP('',(#2611,#2612,#2613,#2614));
#556=EDGE_LOOP('',(#2615,#2616,#2617,#2618));
#557=EDGE_LOOP('',(#2619,#2620,#2621,#2622));
#558=EDGE_LOOP('',(#2623,#2624,#2625,#2626));
#559=EDGE_LOOP('',(#2627,#2628,#2629,#2630));
#560=EDGE_LOOP('',(#2631,#2632,#2633,#2634));
#561=EDGE_LOOP('',(#2635,#2636,#2637,#2638));
#562=EDGE_LOOP('',(#2639,#2640,#2641,#2642));
#563=EDGE_LOOP('',(#2643,#2644,#2645,#2646));
#564=EDGE_LOOP('',(#2647,#2648,#2649,#2650));
#565=EDGE_LOOP('',(#2651,#2652,#2653,#2654));
#566=EDGE_LOOP('',(#2655,#2656,#2657,#2658));
#567=EDGE_LOOP('',(#2659,#2660,#2661,#2662));
#568=EDGE_LOOP('',(#2663,#2664,#2665,#2666));
#569=EDGE_LOOP('',(#2667,#2668,#2669,#2670));
#570=EDGE_LOOP('',(#2671,#2672,#2673,#2674));
#571=EDGE_LOOP('',(#2675,#2676,#2677,#2678));
#572=EDGE_LOOP('',(#2679,#2680,#2681,#2682));
#573=EDGE_LOOP('',(#2683,#2684,#2685,#2686,#2687,#2688,#2689,#2690));
#574=EDGE_LOOP('',(#2691,#2692,#2693,#2694,#2695,#2696,#2697,#2698));
#575=EDGE_LOOP('',(#2699,#2700,#2701,#2702));
#576=EDGE_LOOP('',(#2703,#2704,#2705,#2706));
#577=EDGE_LOOP('',(#2707,#2708,#2709,#2710));
#578=EDGE_LOOP('',(#2711,#2712,#2713,#2714));
#579=EDGE_LOOP('',(#2715,#2716,#2717,#2718));
#580=EDGE_LOOP('',(#2719,#2720,#2721,#2722));
#581=EDGE_LOOP('',(#2723,#2724,#2725,#2726));
#582=EDGE_LOOP('',(#2727,#2728,#2729,#2730));
#583=EDGE_LOOP('',(#2731,#2732,#2733,#2734));
#584=EDGE_LOOP('',(#2735,#2736,#2737,#2738));
#585=EDGE_LOOP('',(#2739,#2740,#2741,#2742));
#586=EDGE_LOOP('',(#2743,#2744,#2745,#2746));
#587=EDGE_LOOP('',(#2747,#2748,#2749,#2750));
#588=EDGE_LOOP('',(#2751,#2752,#2753,#2754));
#589=EDGE_LOOP('',(#2755,#2756,#2757,#2758));
#590=EDGE_LOOP('',(#2759,#2760,#2761,#2762));
#591=EDGE_LOOP('',(#2763,#2764,#2765,#2766));
#592=EDGE_LOOP('',(#2767,#2768,#2769,#2770));
#593=EDGE_LOOP('',(#2771,#2772,#2773,#2774));
#594=EDGE_LOOP('',(#2775,#2776,#2777,#2778));
#595=EDGE_LOOP('',(#2779,#2780,#2781,#2782));
#596=EDGE_LOOP('',(#2783,#2784,#2785,#2786));
#597=EDGE_LOOP('',(#2787,#2788,#2789,#2790));
#598=EDGE_LOOP('',(#2791,#2792,#2793,#2794));
#599=EDGE_LOOP('',(#2795,#2796,#2797,#2798));
#600=EDGE_LOOP('',(#2799,#2800,#2801,#2802));
#601=EDGE_LOOP('',(#2803,#2804,#2805,#2806));
#602=EDGE_LOOP('',(#2807,#2808,#2809,#2810));
#603=EDGE_LOOP('',(#2811,#2812,#2813,#2814));
#604=EDGE_LOOP('',(#2815,#2816,#2817,#2818));
#605=EDGE_LOOP('',(#2819,#2820,#2821,#2822));
#606=EDGE_LOOP('',(#2823,#2824,#2825,#2826));
#607=EDGE_LOOP('',(#2827,#2828,#2829,#2830));
#608=EDGE_LOOP('',(#2831,#2832,#2833,#2834));
#609=EDGE_LOOP('',(#2835,#2836,#2837,#2838));
#610=EDGE_LOOP('',(#2839,#2840,#2841,#2842));
#611=EDGE_LOOP('',(#2843,#2844,#2845,#2846));
#612=EDGE_LOOP('',(#2847,#2848,#2849,#2850));
#613=EDGE_LOOP('',(#2851,#2852,#2853,#2854));
#614=EDGE_LOOP('',(#2855));
#615=EDGE_LOOP('',(#2856,#2857,#2858,#2859));
#616=EDGE_LOOP('',(#2860,#2861,#2862,#2863));
#617=EDGE_LOOP('',(#2864,#2865,#2866,#2867));
#618=EDGE_LOOP('',(#2868,#2869,#2870,#2871));
#619=EDGE_LOOP('',(#2872));
#620=EDGE_LOOP('',(#2873,#2874,#2875,#2876));
#621=EDGE_LOOP('',(#2877,#2878,#2879,#2880));
#622=EDGE_LOOP('',(#2881,#2882,#2883,#2884));
#623=EDGE_LOOP('',(#2885,#2886,#2887,#2888));
#624=EDGE_LOOP('',(#2889));
#625=EDGE_LOOP('',(#2890,#2891,#2892,#2893));
#626=EDGE_LOOP('',(#2894,#2895,#2896,#2897));
#627=EDGE_LOOP('',(#2898,#2899,#2900,#2901));
#628=EDGE_LOOP('',(#2902,#2903,#2904,#2905));
#629=EDGE_LOOP('',(#2906));
#630=EDGE_LOOP('',(#2907,#2908,#2909,#2910));
#631=EDGE_LOOP('',(#2911,#2912,#2913,#2914));
#632=EDGE_LOOP('',(#2915,#2916,#2917,#2918));
#633=EDGE_LOOP('',(#2919,#2920,#2921,#2922));
#634=EDGE_LOOP('',(#2923));
#635=EDGE_LOOP('',(#2924,#2925,#2926,#2927));
#636=EDGE_LOOP('',(#2928,#2929,#2930,#2931));
#637=EDGE_LOOP('',(#2932,#2933,#2934,#2935));
#638=EDGE_LOOP('',(#2936,#2937,#2938,#2939));
#639=EDGE_LOOP('',(#2940));
#640=EDGE_LOOP('',(#2941,#2942,#2943,#2944));
#641=EDGE_LOOP('',(#2945,#2946,#2947,#2948));
#642=EDGE_LOOP('',(#2949,#2950,#2951,#2952,#2953,#2954,#2955,#2956,#2957,
#2958,#2959,#2960,#2961,#2962,#2963,#2964,#2965,#2966,#2967,#2968,#2969,
#2970,#2971,#2972));
#643=EDGE_LOOP('',(#2973,#2974,#2975,#2976,#2977,#2978,#2979,#2980,#2981,
#2982,#2983,#2984,#2985,#2986,#2987,#2988,#2989,#2990,#2991,#2992,#2993,
#2994,#2995,#2996));
#644=EDGE_LOOP('',(#2997,#2998,#2999,#3000));
#645=EDGE_LOOP('',(#3001));
#646=EDGE_LOOP('',(#3002));
#647=LINE('',#4644,#1003);
#648=LINE('',#4646,#1004);
#649=LINE('',#4648,#1005);
#650=LINE('',#4649,#1006);
#651=LINE('',#4653,#1007);
#652=LINE('',#4655,#1008);
#653=LINE('',#4657,#1009);
#654=LINE('',#4658,#1010);
#655=LINE('',#4662,#1011);
#656=LINE('',#4664,#1012);
#657=LINE('',#4666,#1013);
#658=LINE('',#4667,#1014);
#659=LINE('',#4671,#1015);
#660=LINE('',#4673,#1016);
#661=LINE('',#4675,#1017);
#662=LINE('',#4676,#1018);
#663=LINE('',#4680,#1019);
#664=LINE('',#4684,#1020);
#665=LINE('',#4686,#1021);
#666=LINE('',#4688,#1022);
#667=LINE('',#4690,#1023);
#668=LINE('',#4692,#1024);
#669=LINE('',#4694,#1025);
#670=LINE('',#4696,#1026);
#671=LINE('',#4698,#1027);
#672=LINE('',#4700,#1028);
#673=LINE('',#4702,#1029);
#674=LINE('',#4704,#1030);
#675=LINE('',#4706,#1031);
#676=LINE('',#4708,#1032);
#677=LINE('',#4710,#1033);
#678=LINE('',#4712,#1034);
#679=LINE('',#4714,#1035);
#680=LINE('',#4716,#1036);
#681=LINE('',#4718,#1037);
#682=LINE('',#4720,#1038);
#683=LINE('',#4721,#1039);
#684=LINE('',#4726,#1040);
#685=LINE('',#4728,#1041);
#686=LINE('',#4730,#1042);
#687=LINE('',#4734,#1043);
#688=LINE('',#4736,#1044);
#689=LINE('',#4737,#1045);
#690=LINE('',#4742,#1046);
#691=LINE('',#4746,#1047);
#692=LINE('',#4748,#1048);
#693=LINE('',#4750,#1049);
#694=LINE('',#4754,#1050);
#695=LINE('',#4756,#1051);
#696=LINE('',#4758,#1052);
#697=LINE('',#4760,#1053);
#698=LINE('',#4762,#1054);
#699=LINE('',#4764,#1055);
#700=LINE('',#4766,#1056);
#701=LINE('',#4768,#1057);
#702=LINE('',#4770,#1058);
#703=LINE('',#4772,#1059);
#704=LINE('',#4774,#1060);
#705=LINE('',#4776,#1061);
#706=LINE('',#4778,#1062);
#707=LINE('',#4780,#1063);
#708=LINE('',#4782,#1064);
#709=LINE('',#4784,#1065);
#710=LINE('',#4786,#1066);
#711=LINE('',#4788,#1067);
#712=LINE('',#4789,#1068);
#713=LINE('',#4795,#1069);
#714=LINE('',#4798,#1070);
#715=LINE('',#4800,#1071);
#716=LINE('',#4801,#1072);
#717=LINE('',#4807,#1073);
#718=LINE('',#4812,#1074);
#719=LINE('',#4814,#1075);
#720=LINE('',#4816,#1076);
#721=LINE('',#4818,#1077);
#722=LINE('',#4820,#1078);
#723=LINE('',#4822,#1079);
#724=LINE('',#4824,#1080);
#725=LINE('',#4826,#1081);
#726=LINE('',#4828,#1082);
#727=LINE('',#4830,#1083);
#728=LINE('',#4832,#1084);
#729=LINE('',#4834,#1085);
#730=LINE('',#4836,#1086);
#731=LINE('',#4838,#1087);
#732=LINE('',#4840,#1088);
#733=LINE('',#4842,#1089);
#734=LINE('',#4844,#1090);
#735=LINE('',#4846,#1091);
#736=LINE('',#4848,#1092);
#737=LINE('',#4849,#1093);
#738=LINE('',#4853,#1094);
#739=LINE('',#4856,#1095);
#740=LINE('',#4858,#1096);
#741=LINE('',#4862,#1097);
#742=LINE('',#4864,#1098);
#743=LINE('',#4865,#1099);
#744=LINE('',#4871,#1100);
#745=LINE('',#4873,#1101);
#746=LINE('',#4875,#1102);
#747=LINE('',#4879,#1103);
#748=LINE('',#4882,#1104);
#749=LINE('',#4884,#1105);
#750=LINE('',#4886,#1106);
#751=LINE('',#4888,#1107);
#752=LINE('',#4890,#1108);
#753=LINE('',#4892,#1109);
#754=LINE('',#4894,#1110);
#755=LINE('',#4896,#1111);
#756=LINE('',#4898,#1112);
#757=LINE('',#4900,#1113);
#758=LINE('',#4902,#1114);
#759=LINE('',#4904,#1115);
#760=LINE('',#4906,#1116);
#761=LINE('',#4908,#1117);
#762=LINE('',#4910,#1118);
#763=LINE('',#4912,#1119);
#764=LINE('',#4914,#1120);
#765=LINE('',#4916,#1121);
#766=LINE('',#4917,#1122);
#767=LINE('',#4921,#1123);
#768=LINE('',#4927,#1124);
#769=LINE('',#4928,#1125);
#770=LINE('',#4929,#1126);
#771=LINE('',#4934,#1127);
#772=LINE('',#4935,#1128);
#773=LINE('',#4937,#1129);
#774=LINE('',#4938,#1130);
#775=LINE('',#4940,#1131);
#776=LINE('',#4941,#1132);
#777=LINE('',#4943,#1133);
#778=LINE('',#4944,#1134);
#779=LINE('',#4946,#1135);
#780=LINE('',#4947,#1136);
#781=LINE('',#4949,#1137);
#782=LINE('',#4950,#1138);
#783=LINE('',#4952,#1139);
#784=LINE('',#4954,#1140);
#785=LINE('',#4956,#1141);
#786=LINE('',#4957,#1142);
#787=LINE('',#4959,#1143);
#788=LINE('',#4961,#1144);
#789=LINE('',#4963,#1145);
#790=LINE('',#4964,#1146);
#791=LINE('',#4966,#1147);
#792=LINE('',#4967,#1148);
#793=LINE('',#4969,#1149);
#794=LINE('',#4971,#1150);
#795=LINE('',#4973,#1151);
#796=LINE('',#4974,#1152);
#797=LINE('',#4977,#1153);
#798=LINE('',#4978,#1154);
#799=LINE('',#4980,#1155);
#800=LINE('',#4982,#1156);
#801=LINE('',#4983,#1157);
#802=LINE('',#4985,#1158);
#803=LINE('',#4987,#1159);
#804=LINE('',#4989,#1160);
#805=LINE('',#4990,#1161);
#806=LINE('',#4992,#1162);
#807=LINE('',#4993,#1163);
#808=LINE('',#4995,#1164);
#809=LINE('',#4997,#1165);
#810=LINE('',#4999,#1166);
#811=LINE('',#5000,#1167);
#812=LINE('',#5002,#1168);
#813=LINE('',#5004,#1169);
#814=LINE('',#5006,#1170);
#815=LINE('',#5031,#1171);
#816=LINE('',#5035,#1172);
#817=LINE('',#5039,#1173);
#818=LINE('',#5041,#1174);
#819=LINE('',#5042,#1175);
#820=LINE('',#5046,#1176);
#821=LINE('',#5050,#1177);
#822=LINE('',#5054,#1178);
#823=LINE('',#5056,#1179);
#824=LINE('',#5057,#1180);
#825=LINE('',#5061,#1181);
#826=LINE('',#5066,#1182);
#827=LINE('',#5068,#1183);
#828=LINE('',#5069,#1184);
#829=LINE('',#5073,#1185);
#830=LINE('',#5077,#1186);
#831=LINE('',#5080,#1187);
#832=LINE('',#5081,#1188);
#833=LINE('',#5085,#1189);
#834=LINE('',#5090,#1190);
#835=LINE('',#5092,#1191);
#836=LINE('',#5093,#1192);
#837=LINE('',#5097,#1193);
#838=LINE('',#5101,#1194);
#839=LINE('',#5104,#1195);
#840=LINE('',#5105,#1196);
#841=LINE('',#5109,#1197);
#842=LINE('',#5114,#1198);
#843=LINE('',#5116,#1199);
#844=LINE('',#5117,#1200);
#845=LINE('',#5121,#1201);
#846=LINE('',#5125,#1202);
#847=LINE('',#5128,#1203);
#848=LINE('',#5129,#1204);
#849=LINE('',#5132,#1205);
#850=LINE('',#5133,#1206);
#851=LINE('',#5134,#1207);
#852=LINE('',#5137,#1208);
#853=LINE('',#5138,#1209);
#854=LINE('',#5140,#1210);
#855=LINE('',#5141,#1211);
#856=LINE('',#5143,#1212);
#857=LINE('',#5145,#1213);
#858=LINE('',#5147,#1214);
#859=LINE('',#5149,#1215);
#860=LINE('',#5151,#1216);
#861=LINE('',#5153,#1217);
#862=LINE('',#5155,#1218);
#863=LINE('',#5158,#1219);
#864=LINE('',#5159,#1220);
#865=LINE('',#5162,#1221);
#866=LINE('',#5163,#1222);
#867=LINE('',#5165,#1223);
#868=LINE('',#5166,#1224);
#869=LINE('',#5168,#1225);
#870=LINE('',#5170,#1226);
#871=LINE('',#5172,#1227);
#872=LINE('',#5174,#1228);
#873=LINE('',#5176,#1229);
#874=LINE('',#5178,#1230);
#875=LINE('',#5186,#1231);
#876=LINE('',#5188,#1232);
#877=LINE('',#5190,#1233);
#878=LINE('',#5191,#1234);
#879=LINE('',#5194,#1235);
#880=LINE('',#5196,#1236);
#881=LINE('',#5197,#1237);
#882=LINE('',#5200,#1238);
#883=LINE('',#5204,#1239);
#884=LINE('',#5208,#1240);
#885=LINE('',#5212,#1241);
#886=LINE('',#5216,#1242);
#887=LINE('',#5218,#1243);
#888=LINE('',#5219,#1244);
#889=LINE('',#5222,#1245);
#890=LINE('',#5224,#1246);
#891=LINE('',#5225,#1247);
#892=LINE('',#5230,#1248);
#893=LINE('',#5234,#1249);
#894=LINE('',#5236,#1250);
#895=LINE('',#5237,#1251);
#896=LINE('',#5240,#1252);
#897=LINE('',#5242,#1253);
#898=LINE('',#5243,#1254);
#899=LINE('',#5246,#1255);
#900=LINE('',#5250,#1256);
#901=LINE('',#5254,#1257);
#902=LINE('',#5258,#1258);
#903=LINE('',#5266,#1259);
#904=LINE('',#5267,#1260);
#905=LINE('',#5269,#1261);
#906=LINE('',#5271,#1262);
#907=LINE('',#5274,#1263);
#908=LINE('',#5275,#1264);
#909=LINE('',#5277,#1265);
#910=LINE('',#5279,#1266);
#911=LINE('',#5285,#1267);
#912=LINE('',#5289,#1268);
#913=LINE('',#5293,#1269);
#914=LINE('',#5295,#1270);
#915=LINE('',#5296,#1271);
#916=LINE('',#5300,#1272);
#917=LINE('',#5304,#1273);
#918=LINE('',#5308,#1274);
#919=LINE('',#5310,#1275);
#920=LINE('',#5311,#1276);
#921=LINE('',#5314,#1277);
#922=LINE('',#5315,#1278);
#923=LINE('',#5316,#1279);
#924=LINE('',#5319,#1280);
#925=LINE('',#5323,#1281);
#926=LINE('',#5327,#1282);
#927=LINE('',#5331,#1283);
#928=LINE('',#5335,#1284);
#929=LINE('',#5336,#1285);
#930=LINE('',#5338,#1286);
#931=LINE('',#5339,#1287);
#932=LINE('',#5344,#1288);
#933=LINE('',#5347,#1289);
#934=LINE('',#5352,#1290);
#935=LINE('',#5355,#1291);
#936=LINE('',#5357,#1292);
#937=LINE('',#5360,#1293);
#938=LINE('',#5361,#1294);
#939=LINE('',#5364,#1295);
#940=LINE('',#5365,#1296);
#941=LINE('',#5367,#1297);
#942=LINE('',#5368,#1298);
#943=LINE('',#5373,#1299);
#944=LINE('',#5374,#1300);
#945=LINE('',#5376,#1301);
#946=LINE('',#5378,#1302);
#947=LINE('',#5381,#1303);
#948=LINE('',#5382,#1304);
#949=LINE('',#5384,#1305);
#950=LINE('',#5386,#1306);
#951=LINE('',#5393,#1307);
#952=LINE('',#5399,#1308);
#953=LINE('',#5405,#1309);
#954=LINE('',#5412,#1310);
#955=LINE('',#5415,#1311);
#956=LINE('',#5418,#1312);
#957=LINE('',#5420,#1313);
#958=LINE('',#5421,#1314);
#959=LINE('',#5426,#1315);
#960=LINE('',#5430,#1316);
#961=LINE('',#5432,#1317);
#962=LINE('',#5433,#1318);
#963=LINE('',#5438,#1319);
#964=LINE('',#5442,#1320);
#965=LINE('',#5444,#1321);
#966=LINE('',#5445,#1322);
#967=LINE('',#5450,#1323);
#968=LINE('',#5454,#1324);
#969=LINE('',#5456,#1325);
#970=LINE('',#5457,#1326);
#971=LINE('',#5462,#1327);
#972=LINE('',#5466,#1328);
#973=LINE('',#5468,#1329);
#974=LINE('',#5469,#1330);
#975=LINE('',#5474,#1331);
#976=LINE('',#5478,#1332);
#977=LINE('',#5480,#1333);
#978=LINE('',#5481,#1334);
#979=LINE('',#5486,#1335);
#980=LINE('',#5490,#1336);
#981=LINE('',#5492,#1337);
#982=LINE('',#5493,#1338);
#983=LINE('',#5498,#1339);
#984=LINE('',#5502,#1340);
#985=LINE('',#5504,#1341);
#986=LINE('',#5505,#1342);
#987=LINE('',#5510,#1343);
#988=LINE('',#5514,#1344);
#989=LINE('',#5516,#1345);
#990=LINE('',#5517,#1346);
#991=LINE('',#5522,#1347);
#992=LINE('',#5526,#1348);
#993=LINE('',#5528,#1349);
#994=LINE('',#5529,#1350);
#995=LINE('',#5534,#1351);
#996=LINE('',#5538,#1352);
#997=LINE('',#5540,#1353);
#998=LINE('',#5541,#1354);
#999=LINE('',#5546,#1355);
#1000=LINE('',#5549,#1356);
#1001=LINE('',#5550,#1357);
#1002=LINE('',#5558,#1358);
#1003=VECTOR('',#3687,1000.);
#1004=VECTOR('',#3688,1000.);
#1005=VECTOR('',#3689,1000.);
#1006=VECTOR('',#3690,1000.);
#1007=VECTOR('',#3693,1000.);
#1008=VECTOR('',#3694,1000.);
#1009=VECTOR('',#3695,1000.);
#1010=VECTOR('',#3696,1000.);
#1011=VECTOR('',#3699,1000.);
#1012=VECTOR('',#3700,1000.);
#1013=VECTOR('',#3701,1000.);
#1014=VECTOR('',#3702,1000.);
#1015=VECTOR('',#3705,1000.);
#1016=VECTOR('',#3706,1000.);
#1017=VECTOR('',#3707,1000.);
#1018=VECTOR('',#3708,1000.);
#1019=VECTOR('',#3711,1000.);
#1020=VECTOR('',#3714,1000.);
#1021=VECTOR('',#3715,1000.);
#1022=VECTOR('',#3716,1000.);
#1023=VECTOR('',#3717,1000.);
#1024=VECTOR('',#3718,1000.);
#1025=VECTOR('',#3719,1000.);
#1026=VECTOR('',#3720,1000.);
#1027=VECTOR('',#3721,1000.);
#1028=VECTOR('',#3722,1000.);
#1029=VECTOR('',#3723,1000.);
#1030=VECTOR('',#3724,1000.);
#1031=VECTOR('',#3725,1000.);
#1032=VECTOR('',#3726,1000.);
#1033=VECTOR('',#3727,1000.);
#1034=VECTOR('',#3728,1000.);
#1035=VECTOR('',#3729,1000.);
#1036=VECTOR('',#3730,1000.);
#1037=VECTOR('',#3731,1000.);
#1038=VECTOR('',#3732,1000.);
#1039=VECTOR('',#3733,1000.);
#1040=VECTOR('',#3738,1000.);
#1041=VECTOR('',#3739,1000.);
#1042=VECTOR('',#3740,1000.);
#1043=VECTOR('',#3745,1000.);
#1044=VECTOR('',#3746,1000.);
#1045=VECTOR('',#3747,1000.);
#1046=VECTOR('',#3752,1000.);
#1047=VECTOR('',#3755,1000.);
#1048=VECTOR('',#3756,1000.);
#1049=VECTOR('',#3757,1000.);
#1050=VECTOR('',#3762,1000.);
#1051=VECTOR('',#3763,1000.);
#1052=VECTOR('',#3764,1000.);
#1053=VECTOR('',#3765,1000.);
#1054=VECTOR('',#3766,1000.);
#1055=VECTOR('',#3767,1000.);
#1056=VECTOR('',#3768,1000.);
#1057=VECTOR('',#3769,1000.);
#1058=VECTOR('',#3770,1000.);
#1059=VECTOR('',#3771,1000.);
#1060=VECTOR('',#3772,1000.);
#1061=VECTOR('',#3773,1000.);
#1062=VECTOR('',#3774,1000.);
#1063=VECTOR('',#3775,1000.);
#1064=VECTOR('',#3776,1000.);
#1065=VECTOR('',#3777,1000.);
#1066=VECTOR('',#3778,1000.);
#1067=VECTOR('',#3779,1000.);
#1068=VECTOR('',#3780,1000.);
#1069=VECTOR('',#3787,1000.);
#1070=VECTOR('',#3790,1000.);
#1071=VECTOR('',#3791,1000.);
#1072=VECTOR('',#3792,1000.);
#1073=VECTOR('',#3799,1000.);
#1074=VECTOR('',#3804,1000.);
#1075=VECTOR('',#3805,1000.);
#1076=VECTOR('',#3806,1000.);
#1077=VECTOR('',#3807,1000.);
#1078=VECTOR('',#3808,1000.);
#1079=VECTOR('',#3809,1000.);
#1080=VECTOR('',#3810,1000.);
#1081=VECTOR('',#3811,1000.);
#1082=VECTOR('',#3812,1000.);
#1083=VECTOR('',#3813,1000.);
#1084=VECTOR('',#3814,1000.);
#1085=VECTOR('',#3815,1000.);
#1086=VECTOR('',#3816,1000.);
#1087=VECTOR('',#3817,1000.);
#1088=VECTOR('',#3818,1000.);
#1089=VECTOR('',#3819,1000.);
#1090=VECTOR('',#3820,1000.);
#1091=VECTOR('',#3821,1000.);
#1092=VECTOR('',#3822,1000.);
#1093=VECTOR('',#3823,1000.);
#1094=VECTOR('',#3826,1000.);
#1095=VECTOR('',#3829,1000.);
#1096=VECTOR('',#3830,1000.);
#1097=VECTOR('',#3835,1000.);
#1098=VECTOR('',#3836,1000.);
#1099=VECTOR('',#3837,1000.);
#1100=VECTOR('',#3844,1000.);
#1101=VECTOR('',#3845,1000.);
#1102=VECTOR('',#3846,1000.);
#1103=VECTOR('',#3849,1000.);
#1104=VECTOR('',#3852,1000.);
#1105=VECTOR('',#3853,1000.);
#1106=VECTOR('',#3854,1000.);
#1107=VECTOR('',#3855,1000.);
#1108=VECTOR('',#3856,1000.);
#1109=VECTOR('',#3857,1000.);
#1110=VECTOR('',#3858,1000.);
#1111=VECTOR('',#3859,1000.);
#1112=VECTOR('',#3860,1000.);
#1113=VECTOR('',#3861,1000.);
#1114=VECTOR('',#3862,1000.);
#1115=VECTOR('',#3863,1000.);
#1116=VECTOR('',#3864,1000.);
#1117=VECTOR('',#3865,1000.);
#1118=VECTOR('',#3866,1000.);
#1119=VECTOR('',#3867,1000.);
#1120=VECTOR('',#3868,1000.);
#1121=VECTOR('',#3869,1000.);
#1122=VECTOR('',#3870,1000.);
#1123=VECTOR('',#3873,1000.);
#1124=VECTOR('',#3880,1000.);
#1125=VECTOR('',#3881,1000.);
#1126=VECTOR('',#3882,1000.);
#1127=VECTOR('',#3891,1000.);
#1128=VECTOR('',#3892,1000.);
#1129=VECTOR('',#3895,1000.);
#1130=VECTOR('',#3896,1000.);
#1131=VECTOR('',#3899,1000.);
#1132=VECTOR('',#3900,1000.);
#1133=VECTOR('',#3903,1000.);
#1134=VECTOR('',#3904,1000.);
#1135=VECTOR('',#3907,1000.);
#1136=VECTOR('',#3908,1000.);
#1137=VECTOR('',#3911,1000.);
#1138=VECTOR('',#3912,1000.);
#1139=VECTOR('',#3915,1000.);
#1140=VECTOR('',#3918,1000.);
#1141=VECTOR('',#3921,1000.);
#1142=VECTOR('',#3922,1000.);
#1143=VECTOR('',#3925,1000.);
#1144=VECTOR('',#3928,1000.);
#1145=VECTOR('',#3931,1000.);
#1146=VECTOR('',#3932,1000.);
#1147=VECTOR('',#3935,1000.);
#1148=VECTOR('',#3936,1000.);
#1149=VECTOR('',#3939,1000.);
#1150=VECTOR('',#3942,1000.);
#1151=VECTOR('',#3945,1000.);
#1152=VECTOR('',#3946,1000.);
#1153=VECTOR('',#3951,1000.);
#1154=VECTOR('',#3952,1000.);
#1155=VECTOR('',#3955,1000.);
#1156=VECTOR('',#3958,1000.);
#1157=VECTOR('',#3959,1000.);
#1158=VECTOR('',#3962,1000.);
#1159=VECTOR('',#3965,1000.);
#1160=VECTOR('',#3968,1000.);
#1161=VECTOR('',#3969,1000.);
#1162=VECTOR('',#3972,1000.);
#1163=VECTOR('',#3973,1000.);
#1164=VECTOR('',#3976,1000.);
#1165=VECTOR('',#3979,1000.);
#1166=VECTOR('',#3982,1000.);
#1167=VECTOR('',#3983,1000.);
#1168=VECTOR('',#3986,1000.);
#1169=VECTOR('',#3989,1000.);
#1170=VECTOR('',#3992,1000.);
#1171=VECTOR('',#4037,1000.);
#1172=VECTOR('',#4040,1000.);
#1173=VECTOR('',#4045,1000.);
#1174=VECTOR('',#4046,1000.);
#1175=VECTOR('',#4047,1000.);
#1176=VECTOR('',#4050,1000.);
#1177=VECTOR('',#4053,1000.);
#1178=VECTOR('',#4058,1000.);
#1179=VECTOR('',#4059,1000.);
#1180=VECTOR('',#4060,1000.);
#1181=VECTOR('',#4063,1000.);
#1182=VECTOR('',#4070,1000.);
#1183=VECTOR('',#4071,1000.);
#1184=VECTOR('',#4072,1000.);
#1185=VECTOR('',#4075,1000.);
#1186=VECTOR('',#4078,1000.);
#1187=VECTOR('',#4083,1000.);
#1188=VECTOR('',#4084,1000.);
#1189=VECTOR('',#4087,1000.);
#1190=VECTOR('',#4094,1000.);
#1191=VECTOR('',#4095,1000.);
#1192=VECTOR('',#4096,1000.);
#1193=VECTOR('',#4099,1000.);
#1194=VECTOR('',#4102,1000.);
#1195=VECTOR('',#4107,1000.);
#1196=VECTOR('',#4108,1000.);
#1197=VECTOR('',#4111,1000.);
#1198=VECTOR('',#4118,1000.);
#1199=VECTOR('',#4119,1000.);
#1200=VECTOR('',#4120,1000.);
#1201=VECTOR('',#4123,1000.);
#1202=VECTOR('',#4126,1000.);
#1203=VECTOR('',#4131,1000.);
#1204=VECTOR('',#4132,1000.);
#1205=VECTOR('',#4135,1000.);
#1206=VECTOR('',#4136,1000.);
#1207=VECTOR('',#4137,1000.);
#1208=VECTOR('',#4140,1000.);
#1209=VECTOR('',#4141,1000.);
#1210=VECTOR('',#4144,1000.);
#1211=VECTOR('',#4145,1000.);
#1212=VECTOR('',#4148,1000.);
#1213=VECTOR('',#4151,1000.);
#1214=VECTOR('',#4154,1000.);
#1215=VECTOR('',#4157,1000.);
#1216=VECTOR('',#4160,1000.);
#1217=VECTOR('',#4163,1000.);
#1218=VECTOR('',#4166,1000.);
#1219=VECTOR('',#4169,1000.);
#1220=VECTOR('',#4170,1000.);
#1221=VECTOR('',#4173,1000.);
#1222=VECTOR('',#4174,1000.);
#1223=VECTOR('',#4177,1000.);
#1224=VECTOR('',#4178,1000.);
#1225=VECTOR('',#4181,1000.);
#1226=VECTOR('',#4184,1000.);
#1227=VECTOR('',#4187,1000.);
#1228=VECTOR('',#4190,1000.);
#1229=VECTOR('',#4193,1000.);
#1230=VECTOR('',#4196,1000.);
#1231=VECTOR('',#4207,1000.);
#1232=VECTOR('',#4208,1000.);
#1233=VECTOR('',#4209,1000.);
#1234=VECTOR('',#4210,1000.);
#1235=VECTOR('',#4213,1000.);
#1236=VECTOR('',#4214,1000.);
#1237=VECTOR('',#4215,1000.);
#1238=VECTOR('',#4216,1000.);
#1239=VECTOR('',#4219,1000.);
#1240=VECTOR('',#4222,1000.);
#1241=VECTOR('',#4225,1000.);
#1242=VECTOR('',#4230,1000.);
#1243=VECTOR('',#4231,1000.);
#1244=VECTOR('',#4232,1000.);
#1245=VECTOR('',#4235,1000.);
#1246=VECTOR('',#4236,1000.);
#1247=VECTOR('',#4237,1000.);
#1248=VECTOR('',#4242,1000.);
#1249=VECTOR('',#4247,1000.);
#1250=VECTOR('',#4248,1000.);
#1251=VECTOR('',#4249,1000.);
#1252=VECTOR('',#4252,1000.);
#1253=VECTOR('',#4253,1000.);
#1254=VECTOR('',#4254,1000.);
#1255=VECTOR('',#4255,1000.);
#1256=VECTOR('',#4258,1000.);
#1257=VECTOR('',#4261,1000.);
#1258=VECTOR('',#4264,1000.);
#1259=VECTOR('',#4279,1000.);
#1260=VECTOR('',#4280,1000.);
#1261=VECTOR('',#4283,1000.);
#1262=VECTOR('',#4286,1000.);
#1263=VECTOR('',#4291,1000.);
#1264=VECTOR('',#4292,1000.);
#1265=VECTOR('',#4295,1000.);
#1266=VECTOR('',#4298,1000.);
#1267=VECTOR('',#4305,1000.);
#1268=VECTOR('',#4308,1000.);
#1269=VECTOR('',#4313,1000.);
#1270=VECTOR('',#4314,1000.);
#1271=VECTOR('',#4315,1000.);
#1272=VECTOR('',#4318,1000.);
#1273=VECTOR('',#4321,1000.);
#1274=VECTOR('',#4326,1000.);
#1275=VECTOR('',#4327,1000.);
#1276=VECTOR('',#4328,1000.);
#1277=VECTOR('',#4331,1000.);
#1278=VECTOR('',#4332,1000.);
#1279=VECTOR('',#4333,1000.);
#1280=VECTOR('',#4334,1000.);
#1281=VECTOR('',#4337,1000.);
#1282=VECTOR('',#4340,1000.);
#1283=VECTOR('',#4343,1000.);
#1284=VECTOR('',#4348,1000.);
#1285=VECTOR('',#4349,1000.);
#1286=VECTOR('',#4352,1000.);
#1287=VECTOR('',#4353,1000.);
#1288=VECTOR('',#4356,1000.);
#1289=VECTOR('',#4359,1000.);
#1290=VECTOR('',#4362,1000.);
#1291=VECTOR('',#4365,1000.);
#1292=VECTOR('',#4368,1000.);
#1293=VECTOR('',#4371,1000.);
#1294=VECTOR('',#4372,1000.);
#1295=VECTOR('',#4375,1000.);
#1296=VECTOR('',#4376,1000.);
#1297=VECTOR('',#4379,1000.);
#1298=VECTOR('',#4380,1000.);
#1299=VECTOR('',#4389,1000.);
#1300=VECTOR('',#4390,1000.);
#1301=VECTOR('',#4393,1000.);
#1302=VECTOR('',#4396,1000.);
#1303=VECTOR('',#4401,1000.);
#1304=VECTOR('',#4402,1000.);
#1305=VECTOR('',#4405,1000.);
#1306=VECTOR('',#4408,1000.);
#1307=VECTOR('',#4417,0.999999999999991);
#1308=VECTOR('',#4424,0.999999999999991);
#1309=VECTOR('',#4431,1.);
#1310=VECTOR('',#4438,1000.);
#1311=VECTOR('',#4441,1000.);
#1312=VECTOR('',#4444,1000.);
#1313=VECTOR('',#4445,1000.);
#1314=VECTOR('',#4446,1000.);
#1315=VECTOR('',#4451,1000.);
#1316=VECTOR('',#4456,1000.);
#1317=VECTOR('',#4457,1000.);
#1318=VECTOR('',#4458,1000.);
#1319=VECTOR('',#4463,1000.);
#1320=VECTOR('',#4468,1000.);
#1321=VECTOR('',#4469,1000.);
#1322=VECTOR('',#4470,1000.);
#1323=VECTOR('',#4475,1000.);
#1324=VECTOR('',#4480,1000.);
#1325=VECTOR('',#4481,1000.);
#1326=VECTOR('',#4482,1000.);
#1327=VECTOR('',#4487,1000.);
#1328=VECTOR('',#4492,1000.);
#1329=VECTOR('',#4493,1000.);
#1330=VECTOR('',#4494,1000.);
#1331=VECTOR('',#4499,1000.);
#1332=VECTOR('',#4504,1000.);
#1333=VECTOR('',#4505,1000.);
#1334=VECTOR('',#4506,1000.);
#1335=VECTOR('',#4511,1000.);
#1336=VECTOR('',#4516,1000.);
#1337=VECTOR('',#4517,1000.);
#1338=VECTOR('',#4518,1000.);
#1339=VECTOR('',#4523,1000.);
#1340=VECTOR('',#4528,1000.);
#1341=VECTOR('',#4529,1000.);
#1342=VECTOR('',#4530,1000.);
#1343=VECTOR('',#4535,1000.);
#1344=VECTOR('',#4540,1000.);
#1345=VECTOR('',#4541,1000.);
#1346=VECTOR('',#4542,1000.);
#1347=VECTOR('',#4547,1000.);
#1348=VECTOR('',#4552,1000.);
#1349=VECTOR('',#4553,1000.);
#1350=VECTOR('',#4554,1000.);
#1351=VECTOR('',#4559,1000.);
#1352=VECTOR('',#4564,1000.);
#1353=VECTOR('',#4565,1000.);
#1354=VECTOR('',#4566,1000.);
#1355=VECTOR('',#4571,1000.);
#1356=VECTOR('',#4576,1000.);
#1357=VECTOR('',#4577,1000.);
#1358=VECTOR('',#4588,1.);
#1359=VERTEX_POINT('',#4642);
#1360=VERTEX_POINT('',#4643);
#1361=VERTEX_POINT('',#4645);
#1362=VERTEX_POINT('',#4647);
#1363=VERTEX_POINT('',#4651);
#1364=VERTEX_POINT('',#4652);
#1365=VERTEX_POINT('',#4654);
#1366=VERTEX_POINT('',#4656);
#1367=VERTEX_POINT('',#4660);
#1368=VERTEX_POINT('',#4661);
#1369=VERTEX_POINT('',#4663);
#1370=VERTEX_POINT('',#4665);
#1371=VERTEX_POINT('',#4669);
#1372=VERTEX_POINT('',#4670);
#1373=VERTEX_POINT('',#4672);
#1374=VERTEX_POINT('',#4674);
#1375=VERTEX_POINT('',#4678);
#1376=VERTEX_POINT('',#4679);
#1377=VERTEX_POINT('',#4681);
#1378=VERTEX_POINT('',#4683);
#1379=VERTEX_POINT('',#4685);
#1380=VERTEX_POINT('',#4687);
#1381=VERTEX_POINT('',#4689);
#1382=VERTEX_POINT('',#4691);
#1383=VERTEX_POINT('',#4693);
#1384=VERTEX_POINT('',#4695);
#1385=VERTEX_POINT('',#4697);
#1386=VERTEX_POINT('',#4699);
#1387=VERTEX_POINT('',#4701);
#1388=VERTEX_POINT('',#4703);
#1389=VERTEX_POINT('',#4705);
#1390=VERTEX_POINT('',#4707);
#1391=VERTEX_POINT('',#4709);
#1392=VERTEX_POINT('',#4711);
#1393=VERTEX_POINT('',#4713);
#1394=VERTEX_POINT('',#4715);
#1395=VERTEX_POINT('',#4717);
#1396=VERTEX_POINT('',#4719);
#1397=VERTEX_POINT('',#4723);
#1398=VERTEX_POINT('',#4725);
#1399=VERTEX_POINT('',#4727);
#1400=VERTEX_POINT('',#4729);
#1401=VERTEX_POINT('',#4733);
#1402=VERTEX_POINT('',#4735);
#1403=VERTEX_POINT('',#4739);
#1404=VERTEX_POINT('',#4741);
#1405=VERTEX_POINT('',#4743);
#1406=VERTEX_POINT('',#4745);
#1407=VERTEX_POINT('',#4747);
#1408=VERTEX_POINT('',#4749);
#1409=VERTEX_POINT('',#4753);
#1410=VERTEX_POINT('',#4755);
#1411=VERTEX_POINT('',#4757);
#1412=VERTEX_POINT('',#4759);
#1413=VERTEX_POINT('',#4761);
#1414=VERTEX_POINT('',#4763);
#1415=VERTEX_POINT('',#4765);
#1416=VERTEX_POINT('',#4767);
#1417=VERTEX_POINT('',#4769);
#1418=VERTEX_POINT('',#4771);
#1419=VERTEX_POINT('',#4773);
#1420=VERTEX_POINT('',#4775);
#1421=VERTEX_POINT('',#4777);
#1422=VERTEX_POINT('',#4779);
#1423=VERTEX_POINT('',#4781);
#1424=VERTEX_POINT('',#4783);
#1425=VERTEX_POINT('',#4785);
#1426=VERTEX_POINT('',#4787);
#1427=VERTEX_POINT('',#4791);
#1428=VERTEX_POINT('',#4793);
#1429=VERTEX_POINT('',#4797);
#1430=VERTEX_POINT('',#4799);
#1431=VERTEX_POINT('',#4803);
#1432=VERTEX_POINT('',#4805);
#1433=VERTEX_POINT('',#4809);
#1434=VERTEX_POINT('',#4811);
#1435=VERTEX_POINT('',#4813);
#1436=VERTEX_POINT('',#4815);
#1437=VERTEX_POINT('',#4817);
#1438=VERTEX_POINT('',#4819);
#1439=VERTEX_POINT('',#4821);
#1440=VERTEX_POINT('',#4823);
#1441=VERTEX_POINT('',#4825);
#1442=VERTEX_POINT('',#4827);
#1443=VERTEX_POINT('',#4829);
#1444=VERTEX_POINT('',#4831);
#1445=VERTEX_POINT('',#4833);
#1446=VERTEX_POINT('',#4835);
#1447=VERTEX_POINT('',#4837);
#1448=VERTEX_POINT('',#4839);
#1449=VERTEX_POINT('',#4841);
#1450=VERTEX_POINT('',#4843);
#1451=VERTEX_POINT('',#4845);
#1452=VERTEX_POINT('',#4847);
#1453=VERTEX_POINT('',#4850);
#1454=VERTEX_POINT('',#4852);
#1455=VERTEX_POINT('',#4854);
#1456=VERTEX_POINT('',#4857);
#1457=VERTEX_POINT('',#4861);
#1458=VERTEX_POINT('',#4863);
#1459=VERTEX_POINT('',#4868);
#1460=VERTEX_POINT('',#4870);
#1461=VERTEX_POINT('',#4872);
#1462=VERTEX_POINT('',#4874);
#1463=VERTEX_POINT('',#4876);
#1464=VERTEX_POINT('',#4878);
#1465=VERTEX_POINT('',#4881);
#1466=VERTEX_POINT('',#4883);
#1467=VERTEX_POINT('',#4885);
#1468=VERTEX_POINT('',#4887);
#1469=VERTEX_POINT('',#4889);
#1470=VERTEX_POINT('',#4891);
#1471=VERTEX_POINT('',#4893);
#1472=VERTEX_POINT('',#4895);
#1473=VERTEX_POINT('',#4897);
#1474=VERTEX_POINT('',#4899);
#1475=VERTEX_POINT('',#4901);
#1476=VERTEX_POINT('',#4903);
#1477=VERTEX_POINT('',#4905);
#1478=VERTEX_POINT('',#4907);
#1479=VERTEX_POINT('',#4909);
#1480=VERTEX_POINT('',#4911);
#1481=VERTEX_POINT('',#4913);
#1482=VERTEX_POINT('',#4915);
#1483=VERTEX_POINT('',#4919);
#1484=VERTEX_POINT('',#4920);
#1485=VERTEX_POINT('',#4925);
#1486=VERTEX_POINT('',#4926);
#1487=VERTEX_POINT('',#5029);
#1488=VERTEX_POINT('',#5030);
#1489=VERTEX_POINT('',#5032);
#1490=VERTEX_POINT('',#5034);
#1491=VERTEX_POINT('',#5038);
#1492=VERTEX_POINT('',#5040);
#1493=VERTEX_POINT('',#5044);
#1494=VERTEX_POINT('',#5045);
#1495=VERTEX_POINT('',#5047);
#1496=VERTEX_POINT('',#5049);
#1497=VERTEX_POINT('',#5053);
#1498=VERTEX_POINT('',#5055);
#1499=VERTEX_POINT('',#5059);
#1500=VERTEX_POINT('',#5060);
#1501=VERTEX_POINT('',#5065);
#1502=VERTEX_POINT('',#5067);
#1503=VERTEX_POINT('',#5071);
#1504=VERTEX_POINT('',#5072);
#1505=VERTEX_POINT('',#5074);
#1506=VERTEX_POINT('',#5076);
#1507=VERTEX_POINT('',#5083);
#1508=VERTEX_POINT('',#5084);
#1509=VERTEX_POINT('',#5089);
#1510=VERTEX_POINT('',#5091);
#1511=VERTEX_POINT('',#5095);
#1512=VERTEX_POINT('',#5096);
#1513=VERTEX_POINT('',#5098);
#1514=VERTEX_POINT('',#5100);
#1515=VERTEX_POINT('',#5107);
#1516=VERTEX_POINT('',#5108);
#1517=VERTEX_POINT('',#5113);
#1518=VERTEX_POINT('',#5115);
#1519=VERTEX_POINT('',#5119);
#1520=VERTEX_POINT('',#5120);
#1521=VERTEX_POINT('',#5122);
#1522=VERTEX_POINT('',#5124);
#1523=VERTEX_POINT('',#5131);
#1524=VERTEX_POINT('',#5136);
#1525=VERTEX_POINT('',#5157);
#1526=VERTEX_POINT('',#5161);
#1527=VERTEX_POINT('',#5184);
#1528=VERTEX_POINT('',#5185);
#1529=VERTEX_POINT('',#5187);
#1530=VERTEX_POINT('',#5189);
#1531=VERTEX_POINT('',#5193);
#1532=VERTEX_POINT('',#5195);
#1533=VERTEX_POINT('',#5198);
#1534=VERTEX_POINT('',#5199);
#1535=VERTEX_POINT('',#5201);
#1536=VERTEX_POINT('',#5203);
#1537=VERTEX_POINT('',#5206);
#1538=VERTEX_POINT('',#5207);
#1539=VERTEX_POINT('',#5209);
#1540=VERTEX_POINT('',#5211);
#1541=VERTEX_POINT('',#5215);
#1542=VERTEX_POINT('',#5217);
#1543=VERTEX_POINT('',#5221);
#1544=VERTEX_POINT('',#5223);
#1545=VERTEX_POINT('',#5227);
#1546=VERTEX_POINT('',#5229);
#1547=VERTEX_POINT('',#5233);
#1548=VERTEX_POINT('',#5235);
#1549=VERTEX_POINT('',#5239);
#1550=VERTEX_POINT('',#5241);
#1551=VERTEX_POINT('',#5244);
#1552=VERTEX_POINT('',#5245);
#1553=VERTEX_POINT('',#5247);
#1554=VERTEX_POINT('',#5249);
#1555=VERTEX_POINT('',#5252);
#1556=VERTEX_POINT('',#5253);
#1557=VERTEX_POINT('',#5255);
#1558=VERTEX_POINT('',#5257);
#1559=VERTEX_POINT('',#5283);
#1560=VERTEX_POINT('',#5284);
#1561=VERTEX_POINT('',#5286);
#1562=VERTEX_POINT('',#5288);
#1563=VERTEX_POINT('',#5292);
#1564=VERTEX_POINT('',#5294);
#1565=VERTEX_POINT('',#5298);
#1566=VERTEX_POINT('',#5299);
#1567=VERTEX_POINT('',#5301);
#1568=VERTEX_POINT('',#5303);
#1569=VERTEX_POINT('',#5307);
#1570=VERTEX_POINT('',#5309);
#1571=VERTEX_POINT('',#5313);
#1572=VERTEX_POINT('',#5317);
#1573=VERTEX_POINT('',#5318);
#1574=VERTEX_POINT('',#5320);
#1575=VERTEX_POINT('',#5322);
#1576=VERTEX_POINT('',#5325);
#1577=VERTEX_POINT('',#5326);
#1578=VERTEX_POINT('',#5328);
#1579=VERTEX_POINT('',#5330);
#1580=VERTEX_POINT('',#5334);
#1581=VERTEX_POINT('',#5340);
#1582=VERTEX_POINT('',#5341);
#1583=VERTEX_POINT('',#5343);
#1584=VERTEX_POINT('',#5345);
#1585=VERTEX_POINT('',#5348);
#1586=VERTEX_POINT('',#5349);
#1587=VERTEX_POINT('',#5351);
#1588=VERTEX_POINT('',#5353);
#1589=VERTEX_POINT('',#5359);
#1590=VERTEX_POINT('',#5363);
#1591=VERTEX_POINT('',#5390);
#1592=VERTEX_POINT('',#5392);
#1593=VERTEX_POINT('',#5396);
#1594=VERTEX_POINT('',#5398);
#1595=VERTEX_POINT('',#5402);
#1596=VERTEX_POINT('',#5404);
#1597=VERTEX_POINT('',#5408);
#1598=VERTEX_POINT('',#5409);
#1599=VERTEX_POINT('',#5411);
#1600=VERTEX_POINT('',#5413);
#1601=VERTEX_POINT('',#5417);
#1602=VERTEX_POINT('',#5419);
#1603=VERTEX_POINT('',#5423);
#1604=VERTEX_POINT('',#5425);
#1605=VERTEX_POINT('',#5429);
#1606=VERTEX_POINT('',#5431);
#1607=VERTEX_POINT('',#5435);
#1608=VERTEX_POINT('',#5437);
#1609=VERTEX_POINT('',#5441);
#1610=VERTEX_POINT('',#5443);
#1611=VERTEX_POINT('',#5447);
#1612=VERTEX_POINT('',#5449);
#1613=VERTEX_POINT('',#5453);
#1614=VERTEX_POINT('',#5455);
#1615=VERTEX_POINT('',#5459);
#1616=VERTEX_POINT('',#5461);
#1617=VERTEX_POINT('',#5465);
#1618=VERTEX_POINT('',#5467);
#1619=VERTEX_POINT('',#5471);
#1620=VERTEX_POINT('',#5473);
#1621=VERTEX_POINT('',#5477);
#1622=VERTEX_POINT('',#5479);
#1623=VERTEX_POINT('',#5483);
#1624=VERTEX_POINT('',#5485);
#1625=VERTEX_POINT('',#5489);
#1626=VERTEX_POINT('',#5491);
#1627=VERTEX_POINT('',#5495);
#1628=VERTEX_POINT('',#5497);
#1629=VERTEX_POINT('',#5501);
#1630=VERTEX_POINT('',#5503);
#1631=VERTEX_POINT('',#5507);
#1632=VERTEX_POINT('',#5509);
#1633=VERTEX_POINT('',#5513);
#1634=VERTEX_POINT('',#5515);
#1635=VERTEX_POINT('',#5519);
#1636=VERTEX_POINT('',#5521);
#1637=VERTEX_POINT('',#5525);
#1638=VERTEX_POINT('',#5527);
#1639=VERTEX_POINT('',#5531);
#1640=VERTEX_POINT('',#5533);
#1641=VERTEX_POINT('',#5537);
#1642=VERTEX_POINT('',#5539);
#1643=VERTEX_POINT('',#5543);
#1644=VERTEX_POINT('',#5545);
#1645=VERTEX_POINT('',#5555);
#1646=VERTEX_POINT('',#5557);
#1647=EDGE_CURVE('',#1359,#1360,#647,.T.);
#1648=EDGE_CURVE('',#1359,#1361,#648,.T.);
#1649=EDGE_CURVE('',#1361,#1362,#649,.T.);
#1650=EDGE_CURVE('',#1362,#1360,#650,.T.);
#1651=EDGE_CURVE('',#1363,#1364,#651,.T.);
#1652=EDGE_CURVE('',#1363,#1365,#652,.T.);
#1653=EDGE_CURVE('',#1365,#1366,#653,.T.);
#1654=EDGE_CURVE('',#1366,#1364,#654,.T.);
#1655=EDGE_CURVE('',#1367,#1368,#655,.T.);
#1656=EDGE_CURVE('',#1367,#1369,#656,.T.);
#1657=EDGE_CURVE('',#1369,#1370,#657,.T.);
#1658=EDGE_CURVE('',#1370,#1368,#658,.T.);
#1659=EDGE_CURVE('',#1371,#1372,#659,.T.);
#1660=EDGE_CURVE('',#1372,#1373,#660,.T.);
#1661=EDGE_CURVE('',#1374,#1373,#661,.T.);
#1662=EDGE_CURVE('',#1374,#1371,#662,.T.);
#1663=EDGE_CURVE('',#1375,#1376,#663,.T.);
#1664=EDGE_CURVE('',#1376,#1377,#193,.T.);
#1665=EDGE_CURVE('',#1378,#1377,#664,.T.);
#1666=EDGE_CURVE('',#1378,#1379,#665,.T.);
#1667=EDGE_CURVE('',#1379,#1380,#666,.T.);
#1668=EDGE_CURVE('',#1380,#1381,#667,.T.);
#1669=EDGE_CURVE('',#1381,#1382,#668,.T.);
#1670=EDGE_CURVE('',#1382,#1383,#669,.T.);
#1671=EDGE_CURVE('',#1383,#1384,#670,.T.);
#1672=EDGE_CURVE('',#1384,#1385,#671,.T.);
#1673=EDGE_CURVE('',#1385,#1386,#672,.T.);
#1674=EDGE_CURVE('',#1386,#1387,#673,.T.);
#1675=EDGE_CURVE('',#1387,#1388,#674,.T.);
#1676=EDGE_CURVE('',#1388,#1389,#675,.T.);
#1677=EDGE_CURVE('',#1389,#1390,#676,.T.);
#1678=EDGE_CURVE('',#1390,#1391,#677,.T.);
#1679=EDGE_CURVE('',#1391,#1392,#678,.T.);
#1680=EDGE_CURVE('',#1392,#1393,#679,.T.);
#1681=EDGE_CURVE('',#1393,#1394,#680,.T.);
#1682=EDGE_CURVE('',#1394,#1395,#681,.T.);
#1683=EDGE_CURVE('',#1395,#1396,#682,.T.);
#1684=EDGE_CURVE('',#1396,#1362,#683,.T.);
#1685=EDGE_CURVE('',#1361,#1372,#194,.T.);
#1686=EDGE_CURVE('',#1371,#1397,#195,.T.);
#1687=EDGE_CURVE('',#1397,#1398,#684,.T.);
#1688=EDGE_CURVE('',#1398,#1399,#685,.T.);
#1689=EDGE_CURVE('',#1399,#1400,#686,.T.);
#1690=EDGE_CURVE('',#1400,#1375,#196,.T.);
#1691=EDGE_CURVE('',#1377,#1401,#687,.T.);
#1692=EDGE_CURVE('',#1402,#1401,#688,.T.);
#1693=EDGE_CURVE('',#1402,#1378,#689,.T.);
#1694=EDGE_CURVE('',#1401,#1403,#197,.T.);
#1695=EDGE_CURVE('',#1404,#1403,#690,.T.);
#1696=EDGE_CURVE('',#1404,#1405,#198,.T.);
#1697=EDGE_CURVE('',#1405,#1406,#691,.T.);
#1698=EDGE_CURVE('',#1407,#1406,#692,.T.);
#1699=EDGE_CURVE('',#1407,#1408,#693,.T.);
#1700=EDGE_CURVE('',#1408,#1374,#199,.T.);
#1701=EDGE_CURVE('',#1373,#1359,#200,.T.);
#1702=EDGE_CURVE('',#1360,#1409,#694,.T.);
#1703=EDGE_CURVE('',#1409,#1410,#695,.T.);
#1704=EDGE_CURVE('',#1410,#1411,#696,.T.);
#1705=EDGE_CURVE('',#1411,#1412,#697,.T.);
#1706=EDGE_CURVE('',#1412,#1413,#698,.T.);
#1707=EDGE_CURVE('',#1413,#1414,#699,.T.);
#1708=EDGE_CURVE('',#1414,#1415,#700,.T.);
#1709=EDGE_CURVE('',#1415,#1416,#701,.T.);
#1710=EDGE_CURVE('',#1416,#1417,#702,.T.);
#1711=EDGE_CURVE('',#1417,#1418,#703,.T.);
#1712=EDGE_CURVE('',#1418,#1419,#704,.T.);
#1713=EDGE_CURVE('',#1419,#1420,#705,.T.);
#1714=EDGE_CURVE('',#1420,#1421,#706,.T.);
#1715=EDGE_CURVE('',#1421,#1422,#707,.T.);
#1716=EDGE_CURVE('',#1422,#1423,#708,.T.);
#1717=EDGE_CURVE('',#1423,#1424,#709,.T.);
#1718=EDGE_CURVE('',#1424,#1425,#710,.T.);
#1719=EDGE_CURVE('',#1425,#1426,#711,.T.);
#1720=EDGE_CURVE('',#1426,#1402,#712,.T.);
#1721=EDGE_CURVE('',#1407,#1427,#137,.T.);
#1722=EDGE_CURVE('',#1428,#1406,#138,.T.);
#1723=EDGE_CURVE('',#1427,#1428,#713,.T.);
#1724=EDGE_CURVE('',#1427,#1429,#714,.T.);
#1725=EDGE_CURVE('',#1430,#1428,#715,.T.);
#1726=EDGE_CURVE('',#1429,#1430,#716,.T.);
#1727=EDGE_CURVE('',#1429,#1431,#139,.T.);
#1728=EDGE_CURVE('',#1432,#1430,#140,.T.);
#1729=EDGE_CURVE('',#1431,#1432,#717,.T.);
#1730=EDGE_CURVE('',#1369,#1433,#201,.T.);
#1731=EDGE_CURVE('',#1434,#1433,#718,.T.);
#1732=EDGE_CURVE('',#1434,#1435,#719,.T.);
#1733=EDGE_CURVE('',#1436,#1435,#720,.T.);
#1734=EDGE_CURVE('',#1437,#1436,#721,.T.);
#1735=EDGE_CURVE('',#1438,#1437,#722,.T.);
#1736=EDGE_CURVE('',#1438,#1439,#723,.T.);
#1737=EDGE_CURVE('',#1440,#1439,#724,.T.);
#1738=EDGE_CURVE('',#1441,#1440,#725,.T.);
#1739=EDGE_CURVE('',#1442,#1441,#726,.T.);
#1740=EDGE_CURVE('',#1442,#1443,#727,.T.);
#1741=EDGE_CURVE('',#1444,#1443,#728,.T.);
#1742=EDGE_CURVE('',#1444,#1445,#729,.T.);
#1743=EDGE_CURVE('',#1446,#1445,#730,.T.);
#1744=EDGE_CURVE('',#1447,#1446,#731,.T.);
#1745=EDGE_CURVE('',#1448,#1447,#732,.T.);
#1746=EDGE_CURVE('',#1448,#1449,#733,.T.);
#1747=EDGE_CURVE('',#1450,#1449,#734,.T.);
#1748=EDGE_CURVE('',#1451,#1450,#735,.T.);
#1749=EDGE_CURVE('',#1452,#1451,#736,.T.);
#1750=EDGE_CURVE('',#1452,#1366,#737,.T.);
#1751=EDGE_CURVE('',#1365,#1453,#202,.T.);
#1752=EDGE_CURVE('',#1453,#1454,#738,.T.);
#1753=EDGE_CURVE('',#1454,#1455,#203,.T.);
#1754=EDGE_CURVE('',#1431,#1455,#739,.T.);
#1755=EDGE_CURVE('',#1456,#1432,#740,.T.);
#1756=EDGE_CURVE('',#1456,#1370,#204,.T.);
#1757=EDGE_CURVE('',#1433,#1457,#741,.T.);
#1758=EDGE_CURVE('',#1458,#1457,#742,.T.);
#1759=EDGE_CURVE('',#1458,#1434,#743,.T.);
#1760=EDGE_CURVE('',#1457,#1367,#205,.T.);
#1761=EDGE_CURVE('',#1368,#1459,#206,.T.);
#1762=EDGE_CURVE('',#1459,#1460,#744,.T.);
#1763=EDGE_CURVE('',#1461,#1460,#745,.T.);
#1764=EDGE_CURVE('',#1461,#1462,#746,.T.);
#1765=EDGE_CURVE('',#1462,#1463,#207,.T.);
#1766=EDGE_CURVE('',#1464,#1463,#747,.T.);
#1767=EDGE_CURVE('',#1464,#1363,#208,.T.);
#1768=EDGE_CURVE('',#1364,#1465,#748,.T.);
#1769=EDGE_CURVE('',#1465,#1466,#749,.T.);
#1770=EDGE_CURVE('',#1466,#1467,#750,.T.);
#1771=EDGE_CURVE('',#1467,#1468,#751,.T.);
#1772=EDGE_CURVE('',#1468,#1469,#752,.T.);
#1773=EDGE_CURVE('',#1469,#1470,#753,.T.);
#1774=EDGE_CURVE('',#1470,#1471,#754,.T.);
#1775=EDGE_CURVE('',#1471,#1472,#755,.T.);
#1776=EDGE_CURVE('',#1472,#1473,#756,.T.);
#1777=EDGE_CURVE('',#1473,#1474,#757,.T.);
#1778=EDGE_CURVE('',#1474,#1475,#758,.T.);
#1779=EDGE_CURVE('',#1475,#1476,#759,.T.);
#1780=EDGE_CURVE('',#1476,#1477,#760,.T.);
#1781=EDGE_CURVE('',#1477,#1478,#761,.T.);
#1782=EDGE_CURVE('',#1478,#1479,#762,.T.);
#1783=EDGE_CURVE('',#1479,#1480,#763,.T.);
#1784=EDGE_CURVE('',#1480,#1481,#764,.T.);
#1785=EDGE_CURVE('',#1481,#1482,#765,.T.);
#1786=EDGE_CURVE('',#1482,#1458,#766,.T.);
#1787=EDGE_CURVE('',#1483,#1484,#767,.T.);
#1788=EDGE_CURVE('',#1483,#1461,#141,.T.);
#1789=EDGE_CURVE('',#1460,#1484,#142,.T.);
#1790=EDGE_CURVE('',#1485,#1486,#768,.T.);
#1791=EDGE_CURVE('',#1485,#1483,#769,.T.);
#1792=EDGE_CURVE('',#1484,#1486,#770,.T.);
#1793=EDGE_CURVE('',#1398,#1485,#143,.T.);
#1794=EDGE_CURVE('',#1486,#1399,#144,.T.);
#1795=EDGE_CURVE('',#1453,#1464,#771,.T.);
#1796=EDGE_CURVE('',#1463,#1454,#772,.T.);
#1797=EDGE_CURVE('',#1403,#1376,#773,.T.);
#1798=EDGE_CURVE('',#1375,#1404,#774,.T.);
#1799=EDGE_CURVE('',#1459,#1456,#775,.T.);
#1800=EDGE_CURVE('',#1405,#1400,#776,.T.);
#1801=EDGE_CURVE('',#1397,#1408,#777,.T.);
#1802=EDGE_CURVE('',#1455,#1462,#778,.T.);
#1803=EDGE_CURVE('',#1435,#1482,#779,.T.);
#1804=EDGE_CURVE('',#1481,#1436,#780,.T.);
#1805=EDGE_CURVE('',#1465,#1452,#781,.T.);
#1806=EDGE_CURVE('',#1466,#1451,#782,.T.);
#1807=EDGE_CURVE('',#1467,#1450,#783,.T.);
#1808=EDGE_CURVE('',#1449,#1468,#784,.T.);
#1809=EDGE_CURVE('',#1469,#1448,#785,.T.);
#1810=EDGE_CURVE('',#1470,#1447,#786,.T.);
#1811=EDGE_CURVE('',#1471,#1446,#787,.T.);
#1812=EDGE_CURVE('',#1445,#1472,#788,.T.);
#1813=EDGE_CURVE('',#1443,#1474,#789,.T.);
#1814=EDGE_CURVE('',#1473,#1444,#790,.T.);
#1815=EDGE_CURVE('',#1475,#1442,#791,.T.);
#1816=EDGE_CURVE('',#1476,#1441,#792,.T.);
#1817=EDGE_CURVE('',#1477,#1440,#793,.T.);
#1818=EDGE_CURVE('',#1439,#1478,#794,.T.);
#1819=EDGE_CURVE('',#1479,#1438,#795,.T.);
#1820=EDGE_CURVE('',#1480,#1437,#796,.T.);
#1821=EDGE_CURVE('',#1425,#1380,#797,.T.);
#1822=EDGE_CURVE('',#1424,#1381,#798,.T.);
#1823=EDGE_CURVE('',#1423,#1382,#799,.T.);
#1824=EDGE_CURVE('',#1383,#1422,#800,.T.);
#1825=EDGE_CURVE('',#1421,#1384,#801,.T.);
#1826=EDGE_CURVE('',#1420,#1385,#802,.T.);
#1827=EDGE_CURVE('',#1419,#1386,#803,.T.);
#1828=EDGE_CURVE('',#1387,#1418,#804,.T.);
#1829=EDGE_CURVE('',#1417,#1388,#805,.T.);
#1830=EDGE_CURVE('',#1389,#1416,#806,.T.);
#1831=EDGE_CURVE('',#1415,#1390,#807,.T.);
#1832=EDGE_CURVE('',#1414,#1391,#808,.T.);
#1833=EDGE_CURVE('',#1413,#1392,#809,.T.);
#1834=EDGE_CURVE('',#1393,#1412,#810,.T.);
#1835=EDGE_CURVE('',#1411,#1394,#811,.T.);
#1836=EDGE_CURVE('',#1410,#1395,#812,.T.);
#1837=EDGE_CURVE('',#1409,#1396,#813,.T.);
#1838=EDGE_CURVE('',#1379,#1426,#814,.T.);
#1839=EDGE_CURVE('',#1487,#1488,#815,.T.);
#1840=EDGE_CURVE('',#1489,#1487,#209,.T.);
#1841=EDGE_CURVE('',#1490,#1489,#816,.T.);
#1842=EDGE_CURVE('',#1490,#1488,#210,.T.);
#1843=EDGE_CURVE('',#1487,#1491,#817,.T.);
#1844=EDGE_CURVE('',#1488,#1492,#818,.T.);
#1845=EDGE_CURVE('',#1492,#1491,#819,.T.);
#1846=EDGE_CURVE('',#1493,#1494,#820,.T.);
#1847=EDGE_CURVE('',#1493,#1495,#211,.T.);
#1848=EDGE_CURVE('',#1496,#1495,#821,.T.);
#1849=EDGE_CURVE('',#1494,#1496,#212,.T.);
#1850=EDGE_CURVE('',#1497,#1493,#822,.T.);
#1851=EDGE_CURVE('',#1498,#1494,#823,.T.);
#1852=EDGE_CURVE('',#1498,#1497,#824,.T.);
#1853=EDGE_CURVE('',#1499,#1500,#825,.T.);
#1854=EDGE_CURVE('',#1491,#1499,#213,.T.);
#1855=EDGE_CURVE('',#1492,#1500,#214,.T.);
#1856=EDGE_CURVE('',#1499,#1501,#826,.T.);
#1857=EDGE_CURVE('',#1500,#1502,#827,.T.);
#1858=EDGE_CURVE('',#1502,#1501,#828,.T.);
#1859=EDGE_CURVE('',#1503,#1504,#829,.T.);
#1860=EDGE_CURVE('',#1503,#1505,#215,.T.);
#1861=EDGE_CURVE('',#1506,#1505,#830,.T.);
#1862=EDGE_CURVE('',#1504,#1506,#216,.T.);
#1863=EDGE_CURVE('',#1495,#1503,#831,.T.);
#1864=EDGE_CURVE('',#1496,#1504,#832,.T.);
#1865=EDGE_CURVE('',#1507,#1508,#833,.T.);
#1866=EDGE_CURVE('',#1501,#1507,#217,.T.);
#1867=EDGE_CURVE('',#1502,#1508,#218,.T.);
#1868=EDGE_CURVE('',#1507,#1509,#834,.T.);
#1869=EDGE_CURVE('',#1508,#1510,#835,.T.);
#1870=EDGE_CURVE('',#1510,#1509,#836,.T.);
#1871=EDGE_CURVE('',#1511,#1512,#837,.T.);
#1872=EDGE_CURVE('',#1511,#1513,#219,.T.);
#1873=EDGE_CURVE('',#1514,#1513,#838,.T.);
#1874=EDGE_CURVE('',#1512,#1514,#220,.T.);
#1875=EDGE_CURVE('',#1505,#1511,#839,.T.);
#1876=EDGE_CURVE('',#1506,#1512,#840,.T.);
#1877=EDGE_CURVE('',#1515,#1516,#841,.T.);
#1878=EDGE_CURVE('',#1509,#1515,#221,.T.);
#1879=EDGE_CURVE('',#1510,#1516,#222,.T.);
#1880=EDGE_CURVE('',#1515,#1517,#842,.T.);
#1881=EDGE_CURVE('',#1516,#1518,#843,.T.);
#1882=EDGE_CURVE('',#1517,#1518,#844,.T.);
#1883=EDGE_CURVE('',#1519,#1520,#845,.T.);
#1884=EDGE_CURVE('',#1519,#1521,#223,.T.);
#1885=EDGE_CURVE('',#1522,#1521,#846,.T.);
#1886=EDGE_CURVE('',#1520,#1522,#224,.T.);
#1887=EDGE_CURVE('',#1513,#1519,#847,.T.);
#1888=EDGE_CURVE('',#1514,#1520,#848,.T.);
#1889=EDGE_CURVE('',#1522,#1523,#849,.T.);
#1890=EDGE_CURVE('',#1518,#1523,#850,.T.);
#1891=EDGE_CURVE('',#1516,#1522,#851,.T.);
#1892=EDGE_CURVE('',#1524,#1523,#852,.T.);
#1893=EDGE_CURVE('',#1517,#1524,#853,.T.);
#1894=EDGE_CURVE('',#1521,#1524,#854,.T.);
#1895=EDGE_CURVE('',#1515,#1521,#855,.T.);
#1896=EDGE_CURVE('',#1509,#1519,#856,.T.);
#1897=EDGE_CURVE('',#1507,#1513,#857,.T.);
#1898=EDGE_CURVE('',#1501,#1511,#858,.T.);
#1899=EDGE_CURVE('',#1499,#1505,#859,.T.);
#1900=EDGE_CURVE('',#1491,#1503,#860,.T.);
#1901=EDGE_CURVE('',#1487,#1495,#861,.T.);
#1902=EDGE_CURVE('',#1489,#1493,#862,.T.);
#1903=EDGE_CURVE('',#1525,#1497,#863,.T.);
#1904=EDGE_CURVE('',#1525,#1489,#864,.T.);
#1905=EDGE_CURVE('',#1526,#1498,#865,.T.);
#1906=EDGE_CURVE('',#1526,#1525,#866,.T.);
#1907=EDGE_CURVE('',#1490,#1494,#867,.T.);
#1908=EDGE_CURVE('',#1526,#1490,#868,.T.);
#1909=EDGE_CURVE('',#1488,#1496,#869,.T.);
#1910=EDGE_CURVE('',#1492,#1504,#870,.T.);
#1911=EDGE_CURVE('',#1500,#1506,#871,.T.);
#1912=EDGE_CURVE('',#1502,#1512,#872,.T.);
#1913=EDGE_CURVE('',#1508,#1514,#873,.T.);
#1914=EDGE_CURVE('',#1510,#1520,#874,.T.);
#1915=EDGE_CURVE('',#1527,#1528,#875,.T.);
#1916=EDGE_CURVE('',#1529,#1528,#876,.T.);
#1917=EDGE_CURVE('',#1530,#1529,#877,.T.);
#1918=EDGE_CURVE('',#1530,#1527,#878,.T.);
#1919=EDGE_CURVE('',#1528,#1531,#879,.T.);
#1920=EDGE_CURVE('',#1532,#1531,#880,.T.);
#1921=EDGE_CURVE('',#1529,#1532,#881,.T.);
#1922=EDGE_CURVE('',#1533,#1534,#882,.T.);
#1923=EDGE_CURVE('',#1534,#1535,#225,.T.);
#1924=EDGE_CURVE('',#1535,#1536,#883,.T.);
#1925=EDGE_CURVE('',#1536,#1533,#226,.T.);
#1926=EDGE_CURVE('',#1537,#1538,#884,.T.);
#1927=EDGE_CURVE('',#1538,#1539,#227,.T.);
#1928=EDGE_CURVE('',#1539,#1540,#885,.T.);
#1929=EDGE_CURVE('',#1540,#1537,#228,.T.);
#1930=EDGE_CURVE('',#1531,#1541,#886,.T.);
#1931=EDGE_CURVE('',#1542,#1541,#887,.T.);
#1932=EDGE_CURVE('',#1532,#1542,#888,.T.);
#1933=EDGE_CURVE('',#1541,#1543,#889,.T.);
#1934=EDGE_CURVE('',#1544,#1543,#890,.T.);
#1935=EDGE_CURVE('',#1542,#1544,#891,.T.);
#1936=EDGE_CURVE('',#1543,#1545,#229,.T.);
#1937=EDGE_CURVE('',#1546,#1545,#892,.T.);
#1938=EDGE_CURVE('',#1544,#1546,#230,.T.);
#1939=EDGE_CURVE('',#1545,#1547,#893,.T.);
#1940=EDGE_CURVE('',#1548,#1547,#894,.T.);
#1941=EDGE_CURVE('',#1546,#1548,#895,.T.);
#1942=EDGE_CURVE('',#1547,#1549,#896,.T.);
#1943=EDGE_CURVE('',#1550,#1549,#897,.T.);
#1944=EDGE_CURVE('',#1548,#1550,#898,.T.);
#1945=EDGE_CURVE('',#1551,#1552,#899,.T.);
#1946=EDGE_CURVE('',#1553,#1551,#231,.T.);
#1947=EDGE_CURVE('',#1554,#1553,#900,.T.);
#1948=EDGE_CURVE('',#1552,#1554,#232,.T.);
#1949=EDGE_CURVE('',#1555,#1556,#901,.T.);
#1950=EDGE_CURVE('',#1557,#1555,#233,.T.);
#1951=EDGE_CURVE('',#1558,#1557,#902,.T.);
#1952=EDGE_CURVE('',#1556,#1558,#234,.T.);
#1953=EDGE_CURVE('',#1549,#1527,#235,.T.);
#1954=EDGE_CURVE('',#1550,#1530,#236,.T.);
#1955=EDGE_CURVE('',#1538,#1557,#903,.T.);
#1956=EDGE_CURVE('',#1539,#1555,#904,.T.);
#1957=EDGE_CURVE('',#1537,#1558,#905,.T.);
#1958=EDGE_CURVE('',#1540,#1556,#906,.T.);
#1959=EDGE_CURVE('',#1534,#1553,#907,.T.);
#1960=EDGE_CURVE('',#1535,#1551,#908,.T.);
#1961=EDGE_CURVE('',#1533,#1554,#909,.T.);
#1962=EDGE_CURVE('',#1536,#1552,#910,.T.);
#1963=EDGE_CURVE('',#1559,#1560,#911,.T.);
#1964=EDGE_CURVE('',#1561,#1559,#237,.T.);
#1965=EDGE_CURVE('',#1562,#1561,#912,.T.);
#1966=EDGE_CURVE('',#1562,#1560,#238,.T.);
#1967=EDGE_CURVE('',#1559,#1563,#913,.T.);
#1968=EDGE_CURVE('',#1560,#1564,#914,.T.);
#1969=EDGE_CURVE('',#1563,#1564,#915,.T.);
#1970=EDGE_CURVE('',#1565,#1566,#916,.T.);
#1971=EDGE_CURVE('',#1565,#1567,#239,.T.);
#1972=EDGE_CURVE('',#1568,#1567,#917,.T.);
#1973=EDGE_CURVE('',#1566,#1568,#240,.T.);
#1974=EDGE_CURVE('',#1569,#1565,#918,.T.);
#1975=EDGE_CURVE('',#1570,#1566,#919,.T.);
#1976=EDGE_CURVE('',#1570,#1569,#920,.T.);
#1977=EDGE_CURVE('',#1568,#1571,#921,.T.);
#1978=EDGE_CURVE('',#1564,#1571,#922,.T.);
#1979=EDGE_CURVE('',#1560,#1568,#923,.T.);
#1980=EDGE_CURVE('',#1572,#1573,#924,.T.);
#1981=EDGE_CURVE('',#1573,#1574,#241,.T.);
#1982=EDGE_CURVE('',#1574,#1575,#925,.T.);
#1983=EDGE_CURVE('',#1575,#1572,#242,.T.);
#1984=EDGE_CURVE('',#1576,#1577,#926,.T.);
#1985=EDGE_CURVE('',#1577,#1578,#243,.T.);
#1986=EDGE_CURVE('',#1578,#1579,#927,.T.);
#1987=EDGE_CURVE('',#1579,#1576,#244,.T.);
#1988=EDGE_CURVE('',#1580,#1571,#928,.T.);
#1989=EDGE_CURVE('',#1563,#1580,#929,.T.);
#1990=EDGE_CURVE('',#1567,#1580,#930,.T.);
#1991=EDGE_CURVE('',#1559,#1567,#931,.T.);
#1992=EDGE_CURVE('',#1581,#1582,#245,.T.);
#1993=EDGE_CURVE('',#1583,#1581,#932,.T.);
#1994=EDGE_CURVE('',#1584,#1583,#246,.T.);
#1995=EDGE_CURVE('',#1582,#1584,#933,.T.);
#1996=EDGE_CURVE('',#1585,#1586,#247,.T.);
#1997=EDGE_CURVE('',#1587,#1585,#934,.T.);
#1998=EDGE_CURVE('',#1588,#1587,#248,.T.);
#1999=EDGE_CURVE('',#1586,#1588,#935,.T.);
#2000=EDGE_CURVE('',#1561,#1565,#936,.T.);
#2001=EDGE_CURVE('',#1589,#1569,#937,.T.);
#2002=EDGE_CURVE('',#1589,#1561,#938,.T.);
#2003=EDGE_CURVE('',#1590,#1570,#939,.T.);
#2004=EDGE_CURVE('',#1590,#1589,#940,.T.);
#2005=EDGE_CURVE('',#1562,#1566,#941,.T.);
#2006=EDGE_CURVE('',#1590,#1562,#942,.T.);
#2007=EDGE_CURVE('',#1577,#1585,#943,.T.);
#2008=EDGE_CURVE('',#1578,#1586,#944,.T.);
#2009=EDGE_CURVE('',#1576,#1587,#945,.T.);
#2010=EDGE_CURVE('',#1579,#1588,#946,.T.);
#2011=EDGE_CURVE('',#1573,#1581,#947,.T.);
#2012=EDGE_CURVE('',#1574,#1582,#948,.T.);
#2013=EDGE_CURVE('',#1572,#1583,#949,.T.);
#2014=EDGE_CURVE('',#1575,#1584,#950,.T.);
#2015=EDGE_CURVE('',#1591,#1591,#249,.T.);
#2016=EDGE_CURVE('',#1591,#1592,#951,.T.);
#2017=EDGE_CURVE('',#1592,#1592,#250,.T.);
#2018=EDGE_CURVE('',#1593,#1593,#251,.T.);
#2019=EDGE_CURVE('',#1593,#1594,#952,.T.);
#2020=EDGE_CURVE('',#1594,#1594,#252,.T.);
#2021=EDGE_CURVE('',#1595,#1595,#253,.T.);
#2022=EDGE_CURVE('',#1595,#1596,#953,.T.);
#2023=EDGE_CURVE('',#1596,#1596,#254,.T.);
#2024=EDGE_CURVE('',#1597,#1598,#255,.T.);
#2025=EDGE_CURVE('',#1599,#1598,#954,.T.);
#2026=EDGE_CURVE('',#1600,#1599,#256,.T.);
#2027=EDGE_CURVE('',#1600,#1597,#955,.T.);
#2028=EDGE_CURVE('',#1598,#1601,#956,.T.);
#2029=EDGE_CURVE('',#1602,#1601,#957,.T.);
#2030=EDGE_CURVE('',#1599,#1602,#958,.T.);
#2031=EDGE_CURVE('',#1601,#1603,#257,.T.);
#2032=EDGE_CURVE('',#1604,#1603,#959,.T.);
#2033=EDGE_CURVE('',#1602,#1604,#258,.T.);
#2034=EDGE_CURVE('',#1603,#1605,#960,.T.);
#2035=EDGE_CURVE('',#1606,#1605,#961,.T.);
#2036=EDGE_CURVE('',#1604,#1606,#962,.T.);
#2037=EDGE_CURVE('',#1605,#1607,#259,.T.);
#2038=EDGE_CURVE('',#1608,#1607,#963,.T.);
#2039=EDGE_CURVE('',#1606,#1608,#260,.T.);
#2040=EDGE_CURVE('',#1607,#1609,#964,.T.);
#2041=EDGE_CURVE('',#1610,#1609,#965,.T.);
#2042=EDGE_CURVE('',#1608,#1610,#966,.T.);
#2043=EDGE_CURVE('',#1609,#1611,#261,.T.);
#2044=EDGE_CURVE('',#1612,#1611,#967,.T.);
#2045=EDGE_CURVE('',#1610,#1612,#262,.T.);
#2046=EDGE_CURVE('',#1611,#1613,#968,.T.);
#2047=EDGE_CURVE('',#1614,#1613,#969,.T.);
#2048=EDGE_CURVE('',#1612,#1614,#970,.T.);
#2049=EDGE_CURVE('',#1613,#1615,#263,.T.);
#2050=EDGE_CURVE('',#1616,#1615,#971,.T.);
#2051=EDGE_CURVE('',#1614,#1616,#264,.T.);
#2052=EDGE_CURVE('',#1615,#1617,#972,.T.);
#2053=EDGE_CURVE('',#1618,#1617,#973,.T.);
#2054=EDGE_CURVE('',#1616,#1618,#974,.T.);
#2055=EDGE_CURVE('',#1617,#1619,#265,.T.);
#2056=EDGE_CURVE('',#1620,#1619,#975,.T.);
#2057=EDGE_CURVE('',#1618,#1620,#266,.T.);
#2058=EDGE_CURVE('',#1619,#1621,#976,.T.);
#2059=EDGE_CURVE('',#1622,#1621,#977,.T.);
#2060=EDGE_CURVE('',#1620,#1622,#978,.T.);
#2061=EDGE_CURVE('',#1621,#1623,#267,.T.);
#2062=EDGE_CURVE('',#1624,#1623,#979,.T.);
#2063=EDGE_CURVE('',#1622,#1624,#268,.T.);
#2064=EDGE_CURVE('',#1623,#1625,#980,.T.);
#2065=EDGE_CURVE('',#1626,#1625,#981,.T.);
#2066=EDGE_CURVE('',#1624,#1626,#982,.T.);
#2067=EDGE_CURVE('',#1625,#1627,#269,.T.);
#2068=EDGE_CURVE('',#1628,#1627,#983,.T.);
#2069=EDGE_CURVE('',#1626,#1628,#270,.T.);
#2070=EDGE_CURVE('',#1627,#1629,#984,.T.);
#2071=EDGE_CURVE('',#1630,#1629,#985,.T.);
#2072=EDGE_CURVE('',#1628,#1630,#986,.T.);
#2073=EDGE_CURVE('',#1629,#1631,#271,.T.);
#2074=EDGE_CURVE('',#1632,#1631,#987,.T.);
#2075=EDGE_CURVE('',#1630,#1632,#272,.T.);
#2076=EDGE_CURVE('',#1631,#1633,#988,.T.);
#2077=EDGE_CURVE('',#1634,#1633,#989,.T.);
#2078=EDGE_CURVE('',#1632,#1634,#990,.T.);
#2079=EDGE_CURVE('',#1633,#1635,#273,.T.);
#2080=EDGE_CURVE('',#1636,#1635,#991,.T.);
#2081=EDGE_CURVE('',#1634,#1636,#274,.T.);
#2082=EDGE_CURVE('',#1635,#1637,#992,.T.);
#2083=EDGE_CURVE('',#1638,#1637,#993,.T.);
#2084=EDGE_CURVE('',#1636,#1638,#994,.T.);
#2085=EDGE_CURVE('',#1637,#1639,#275,.T.);
#2086=EDGE_CURVE('',#1640,#1639,#995,.T.);
#2087=EDGE_CURVE('',#1638,#1640,#276,.T.);
#2088=EDGE_CURVE('',#1639,#1641,#996,.T.);
#2089=EDGE_CURVE('',#1642,#1641,#997,.T.);
#2090=EDGE_CURVE('',#1640,#1642,#998,.T.);
#2091=EDGE_CURVE('',#1641,#1643,#277,.T.);
#2092=EDGE_CURVE('',#1644,#1643,#999,.T.);
#2093=EDGE_CURVE('',#1642,#1644,#278,.T.);
#2094=EDGE_CURVE('',#1643,#1597,#1000,.T.);
#2095=EDGE_CURVE('',#1644,#1600,#1001,.T.);
#2096=EDGE_CURVE('',#1645,#1645,#279,.T.);
#2097=EDGE_CURVE('',#1645,#1646,#1002,.T.);
#2098=EDGE_CURVE('',#1646,#1646,#280,.T.);
#2099=ORIENTED_EDGE('',*,*,#1647,.F.);
#2100=ORIENTED_EDGE('',*,*,#1648,.T.);
#2101=ORIENTED_EDGE('',*,*,#1649,.T.);
#2102=ORIENTED_EDGE('',*,*,#1650,.T.);
#2103=ORIENTED_EDGE('',*,*,#1651,.F.);
#2104=ORIENTED_EDGE('',*,*,#1652,.T.);
#2105=ORIENTED_EDGE('',*,*,#1653,.T.);
#2106=ORIENTED_EDGE('',*,*,#1654,.T.);
#2107=ORIENTED_EDGE('',*,*,#1655,.F.);
#2108=ORIENTED_EDGE('',*,*,#1656,.T.);
#2109=ORIENTED_EDGE('',*,*,#1657,.T.);
#2110=ORIENTED_EDGE('',*,*,#1658,.T.);
#2111=ORIENTED_EDGE('',*,*,#1659,.T.);
#2112=ORIENTED_EDGE('',*,*,#1660,.T.);
#2113=ORIENTED_EDGE('',*,*,#1661,.F.);
#2114=ORIENTED_EDGE('',*,*,#1662,.T.);
#2115=ORIENTED_EDGE('',*,*,#1663,.T.);
#2116=ORIENTED_EDGE('',*,*,#1664,.T.);
#2117=ORIENTED_EDGE('',*,*,#1665,.F.);
#2118=ORIENTED_EDGE('',*,*,#1666,.T.);
#2119=ORIENTED_EDGE('',*,*,#1667,.T.);
#2120=ORIENTED_EDGE('',*,*,#1668,.T.);
#2121=ORIENTED_EDGE('',*,*,#1669,.T.);
#2122=ORIENTED_EDGE('',*,*,#1670,.T.);
#2123=ORIENTED_EDGE('',*,*,#1671,.T.);
#2124=ORIENTED_EDGE('',*,*,#1672,.T.);
#2125=ORIENTED_EDGE('',*,*,#1673,.T.);
#2126=ORIENTED_EDGE('',*,*,#1674,.T.);
#2127=ORIENTED_EDGE('',*,*,#1675,.T.);
#2128=ORIENTED_EDGE('',*,*,#1676,.T.);
#2129=ORIENTED_EDGE('',*,*,#1677,.T.);
#2130=ORIENTED_EDGE('',*,*,#1678,.T.);
#2131=ORIENTED_EDGE('',*,*,#1679,.T.);
#2132=ORIENTED_EDGE('',*,*,#1680,.T.);
#2133=ORIENTED_EDGE('',*,*,#1681,.T.);
#2134=ORIENTED_EDGE('',*,*,#1682,.T.);
#2135=ORIENTED_EDGE('',*,*,#1683,.T.);
#2136=ORIENTED_EDGE('',*,*,#1684,.T.);
#2137=ORIENTED_EDGE('',*,*,#1649,.F.);
#2138=ORIENTED_EDGE('',*,*,#1685,.T.);
#2139=ORIENTED_EDGE('',*,*,#1659,.F.);
#2140=ORIENTED_EDGE('',*,*,#1686,.T.);
#2141=ORIENTED_EDGE('',*,*,#1687,.T.);
#2142=ORIENTED_EDGE('',*,*,#1688,.T.);
#2143=ORIENTED_EDGE('',*,*,#1689,.T.);
#2144=ORIENTED_EDGE('',*,*,#1690,.T.);
#2145=ORIENTED_EDGE('',*,*,#1665,.T.);
#2146=ORIENTED_EDGE('',*,*,#1691,.T.);
#2147=ORIENTED_EDGE('',*,*,#1692,.F.);
#2148=ORIENTED_EDGE('',*,*,#1693,.T.);
#2149=ORIENTED_EDGE('',*,*,#1692,.T.);
#2150=ORIENTED_EDGE('',*,*,#1694,.T.);
#2151=ORIENTED_EDGE('',*,*,#1695,.F.);
#2152=ORIENTED_EDGE('',*,*,#1696,.T.);
#2153=ORIENTED_EDGE('',*,*,#1697,.T.);
#2154=ORIENTED_EDGE('',*,*,#1698,.F.);
#2155=ORIENTED_EDGE('',*,*,#1699,.T.);
#2156=ORIENTED_EDGE('',*,*,#1700,.T.);
#2157=ORIENTED_EDGE('',*,*,#1661,.T.);
#2158=ORIENTED_EDGE('',*,*,#1701,.T.);
#2159=ORIENTED_EDGE('',*,*,#1647,.T.);
#2160=ORIENTED_EDGE('',*,*,#1702,.T.);
#2161=ORIENTED_EDGE('',*,*,#1703,.T.);
#2162=ORIENTED_EDGE('',*,*,#1704,.T.);
#2163=ORIENTED_EDGE('',*,*,#1705,.T.);
#2164=ORIENTED_EDGE('',*,*,#1706,.T.);
#2165=ORIENTED_EDGE('',*,*,#1707,.T.);
#2166=ORIENTED_EDGE('',*,*,#1708,.T.);
#2167=ORIENTED_EDGE('',*,*,#1709,.T.);
#2168=ORIENTED_EDGE('',*,*,#1710,.T.);
#2169=ORIENTED_EDGE('',*,*,#1711,.T.);
#2170=ORIENTED_EDGE('',*,*,#1712,.T.);
#2171=ORIENTED_EDGE('',*,*,#1713,.T.);
#2172=ORIENTED_EDGE('',*,*,#1714,.T.);
#2173=ORIENTED_EDGE('',*,*,#1715,.T.);
#2174=ORIENTED_EDGE('',*,*,#1716,.T.);
#2175=ORIENTED_EDGE('',*,*,#1717,.T.);
#2176=ORIENTED_EDGE('',*,*,#1718,.T.);
#2177=ORIENTED_EDGE('',*,*,#1719,.T.);
#2178=ORIENTED_EDGE('',*,*,#1720,.T.);
#2179=ORIENTED_EDGE('',*,*,#1721,.F.);
#2180=ORIENTED_EDGE('',*,*,#1698,.T.);
#2181=ORIENTED_EDGE('',*,*,#1722,.F.);
#2182=ORIENTED_EDGE('',*,*,#1723,.F.);
#2183=ORIENTED_EDGE('',*,*,#1724,.F.);
#2184=ORIENTED_EDGE('',*,*,#1723,.T.);
#2185=ORIENTED_EDGE('',*,*,#1725,.F.);
#2186=ORIENTED_EDGE('',*,*,#1726,.F.);
#2187=ORIENTED_EDGE('',*,*,#1727,.F.);
#2188=ORIENTED_EDGE('',*,*,#1726,.T.);
#2189=ORIENTED_EDGE('',*,*,#1728,.F.);
#2190=ORIENTED_EDGE('',*,*,#1729,.F.);
#2191=ORIENTED_EDGE('',*,*,#1657,.F.);
#2192=ORIENTED_EDGE('',*,*,#1730,.T.);
#2193=ORIENTED_EDGE('',*,*,#1731,.F.);
#2194=ORIENTED_EDGE('',*,*,#1732,.T.);
#2195=ORIENTED_EDGE('',*,*,#1733,.F.);
#2196=ORIENTED_EDGE('',*,*,#1734,.F.);
#2197=ORIENTED_EDGE('',*,*,#1735,.F.);
#2198=ORIENTED_EDGE('',*,*,#1736,.T.);
#2199=ORIENTED_EDGE('',*,*,#1737,.F.);
#2200=ORIENTED_EDGE('',*,*,#1738,.F.);
#2201=ORIENTED_EDGE('',*,*,#1739,.F.);
#2202=ORIENTED_EDGE('',*,*,#1740,.T.);
#2203=ORIENTED_EDGE('',*,*,#1741,.F.);
#2204=ORIENTED_EDGE('',*,*,#1742,.T.);
#2205=ORIENTED_EDGE('',*,*,#1743,.F.);
#2206=ORIENTED_EDGE('',*,*,#1744,.F.);
#2207=ORIENTED_EDGE('',*,*,#1745,.F.);
#2208=ORIENTED_EDGE('',*,*,#1746,.T.);
#2209=ORIENTED_EDGE('',*,*,#1747,.F.);
#2210=ORIENTED_EDGE('',*,*,#1748,.F.);
#2211=ORIENTED_EDGE('',*,*,#1749,.F.);
#2212=ORIENTED_EDGE('',*,*,#1750,.T.);
#2213=ORIENTED_EDGE('',*,*,#1653,.F.);
#2214=ORIENTED_EDGE('',*,*,#1751,.T.);
#2215=ORIENTED_EDGE('',*,*,#1752,.T.);
#2216=ORIENTED_EDGE('',*,*,#1753,.T.);
#2217=ORIENTED_EDGE('',*,*,#1754,.F.);
#2218=ORIENTED_EDGE('',*,*,#1729,.T.);
#2219=ORIENTED_EDGE('',*,*,#1755,.F.);
#2220=ORIENTED_EDGE('',*,*,#1756,.T.);
#2221=ORIENTED_EDGE('',*,*,#1731,.T.);
#2222=ORIENTED_EDGE('',*,*,#1757,.T.);
#2223=ORIENTED_EDGE('',*,*,#1758,.F.);
#2224=ORIENTED_EDGE('',*,*,#1759,.T.);
#2225=ORIENTED_EDGE('',*,*,#1758,.T.);
#2226=ORIENTED_EDGE('',*,*,#1760,.T.);
#2227=ORIENTED_EDGE('',*,*,#1655,.T.);
#2228=ORIENTED_EDGE('',*,*,#1761,.T.);
#2229=ORIENTED_EDGE('',*,*,#1762,.T.);
#2230=ORIENTED_EDGE('',*,*,#1763,.F.);
#2231=ORIENTED_EDGE('',*,*,#1764,.T.);
#2232=ORIENTED_EDGE('',*,*,#1765,.T.);
#2233=ORIENTED_EDGE('',*,*,#1766,.F.);
#2234=ORIENTED_EDGE('',*,*,#1767,.T.);
#2235=ORIENTED_EDGE('',*,*,#1651,.T.);
#2236=ORIENTED_EDGE('',*,*,#1768,.T.);
#2237=ORIENTED_EDGE('',*,*,#1769,.T.);
#2238=ORIENTED_EDGE('',*,*,#1770,.T.);
#2239=ORIENTED_EDGE('',*,*,#1771,.T.);
#2240=ORIENTED_EDGE('',*,*,#1772,.T.);
#2241=ORIENTED_EDGE('',*,*,#1773,.T.);
#2242=ORIENTED_EDGE('',*,*,#1774,.T.);
#2243=ORIENTED_EDGE('',*,*,#1775,.T.);
#2244=ORIENTED_EDGE('',*,*,#1776,.T.);
#2245=ORIENTED_EDGE('',*,*,#1777,.T.);
#2246=ORIENTED_EDGE('',*,*,#1778,.T.);
#2247=ORIENTED_EDGE('',*,*,#1779,.T.);
#2248=ORIENTED_EDGE('',*,*,#1780,.T.);
#2249=ORIENTED_EDGE('',*,*,#1781,.T.);
#2250=ORIENTED_EDGE('',*,*,#1782,.T.);
#2251=ORIENTED_EDGE('',*,*,#1783,.T.);
#2252=ORIENTED_EDGE('',*,*,#1784,.T.);
#2253=ORIENTED_EDGE('',*,*,#1785,.T.);
#2254=ORIENTED_EDGE('',*,*,#1786,.T.);
#2255=ORIENTED_EDGE('',*,*,#1787,.F.);
#2256=ORIENTED_EDGE('',*,*,#1788,.T.);
#2257=ORIENTED_EDGE('',*,*,#1763,.T.);
#2258=ORIENTED_EDGE('',*,*,#1789,.T.);
#2259=ORIENTED_EDGE('',*,*,#1790,.F.);
#2260=ORIENTED_EDGE('',*,*,#1791,.T.);
#2261=ORIENTED_EDGE('',*,*,#1787,.T.);
#2262=ORIENTED_EDGE('',*,*,#1792,.T.);
#2263=ORIENTED_EDGE('',*,*,#1688,.F.);
#2264=ORIENTED_EDGE('',*,*,#1793,.T.);
#2265=ORIENTED_EDGE('',*,*,#1790,.T.);
#2266=ORIENTED_EDGE('',*,*,#1794,.T.);
#2267=ORIENTED_EDGE('',*,*,#1752,.F.);
#2268=ORIENTED_EDGE('',*,*,#1795,.T.);
#2269=ORIENTED_EDGE('',*,*,#1766,.T.);
#2270=ORIENTED_EDGE('',*,*,#1796,.T.);
#2271=ORIENTED_EDGE('',*,*,#1695,.T.);
#2272=ORIENTED_EDGE('',*,*,#1797,.T.);
#2273=ORIENTED_EDGE('',*,*,#1663,.F.);
#2274=ORIENTED_EDGE('',*,*,#1798,.T.);
#2275=ORIENTED_EDGE('',*,*,#1762,.F.);
#2276=ORIENTED_EDGE('',*,*,#1799,.T.);
#2277=ORIENTED_EDGE('',*,*,#1755,.T.);
#2278=ORIENTED_EDGE('',*,*,#1728,.T.);
#2279=ORIENTED_EDGE('',*,*,#1725,.T.);
#2280=ORIENTED_EDGE('',*,*,#1722,.T.);
#2281=ORIENTED_EDGE('',*,*,#1697,.F.);
#2282=ORIENTED_EDGE('',*,*,#1800,.T.);
#2283=ORIENTED_EDGE('',*,*,#1689,.F.);
#2284=ORIENTED_EDGE('',*,*,#1794,.F.);
#2285=ORIENTED_EDGE('',*,*,#1792,.F.);
#2286=ORIENTED_EDGE('',*,*,#1789,.F.);
#2287=ORIENTED_EDGE('',*,*,#1687,.F.);
#2288=ORIENTED_EDGE('',*,*,#1801,.T.);
#2289=ORIENTED_EDGE('',*,*,#1699,.F.);
#2290=ORIENTED_EDGE('',*,*,#1721,.T.);
#2291=ORIENTED_EDGE('',*,*,#1724,.T.);
#2292=ORIENTED_EDGE('',*,*,#1727,.T.);
#2293=ORIENTED_EDGE('',*,*,#1754,.T.);
#2294=ORIENTED_EDGE('',*,*,#1802,.T.);
#2295=ORIENTED_EDGE('',*,*,#1764,.F.);
#2296=ORIENTED_EDGE('',*,*,#1788,.F.);
#2297=ORIENTED_EDGE('',*,*,#1791,.F.);
#2298=ORIENTED_EDGE('',*,*,#1793,.F.);
#2299=ORIENTED_EDGE('',*,*,#1733,.T.);
#2300=ORIENTED_EDGE('',*,*,#1803,.T.);
#2301=ORIENTED_EDGE('',*,*,#1785,.F.);
#2302=ORIENTED_EDGE('',*,*,#1804,.T.);
#2303=ORIENTED_EDGE('',*,*,#1769,.F.);
#2304=ORIENTED_EDGE('',*,*,#1805,.T.);
#2305=ORIENTED_EDGE('',*,*,#1749,.T.);
#2306=ORIENTED_EDGE('',*,*,#1806,.F.);
#2307=ORIENTED_EDGE('',*,*,#1806,.T.);
#2308=ORIENTED_EDGE('',*,*,#1748,.T.);
#2309=ORIENTED_EDGE('',*,*,#1807,.F.);
#2310=ORIENTED_EDGE('',*,*,#1770,.F.);
#2311=ORIENTED_EDGE('',*,*,#1747,.T.);
#2312=ORIENTED_EDGE('',*,*,#1808,.T.);
#2313=ORIENTED_EDGE('',*,*,#1771,.F.);
#2314=ORIENTED_EDGE('',*,*,#1807,.T.);
#2315=ORIENTED_EDGE('',*,*,#1773,.F.);
#2316=ORIENTED_EDGE('',*,*,#1809,.T.);
#2317=ORIENTED_EDGE('',*,*,#1745,.T.);
#2318=ORIENTED_EDGE('',*,*,#1810,.F.);
#2319=ORIENTED_EDGE('',*,*,#1810,.T.);
#2320=ORIENTED_EDGE('',*,*,#1744,.T.);
#2321=ORIENTED_EDGE('',*,*,#1811,.F.);
#2322=ORIENTED_EDGE('',*,*,#1774,.F.);
#2323=ORIENTED_EDGE('',*,*,#1743,.T.);
#2324=ORIENTED_EDGE('',*,*,#1812,.T.);
#2325=ORIENTED_EDGE('',*,*,#1775,.F.);
#2326=ORIENTED_EDGE('',*,*,#1811,.T.);
#2327=ORIENTED_EDGE('',*,*,#1741,.T.);
#2328=ORIENTED_EDGE('',*,*,#1813,.T.);
#2329=ORIENTED_EDGE('',*,*,#1777,.F.);
#2330=ORIENTED_EDGE('',*,*,#1814,.T.);
#2331=ORIENTED_EDGE('',*,*,#1779,.F.);
#2332=ORIENTED_EDGE('',*,*,#1815,.T.);
#2333=ORIENTED_EDGE('',*,*,#1739,.T.);
#2334=ORIENTED_EDGE('',*,*,#1816,.F.);
#2335=ORIENTED_EDGE('',*,*,#1816,.T.);
#2336=ORIENTED_EDGE('',*,*,#1738,.T.);
#2337=ORIENTED_EDGE('',*,*,#1817,.F.);
#2338=ORIENTED_EDGE('',*,*,#1780,.F.);
#2339=ORIENTED_EDGE('',*,*,#1737,.T.);
#2340=ORIENTED_EDGE('',*,*,#1818,.T.);
#2341=ORIENTED_EDGE('',*,*,#1781,.F.);
#2342=ORIENTED_EDGE('',*,*,#1817,.T.);
#2343=ORIENTED_EDGE('',*,*,#1783,.F.);
#2344=ORIENTED_EDGE('',*,*,#1819,.T.);
#2345=ORIENTED_EDGE('',*,*,#1735,.T.);
#2346=ORIENTED_EDGE('',*,*,#1820,.F.);
#2347=ORIENTED_EDGE('',*,*,#1820,.T.);
#2348=ORIENTED_EDGE('',*,*,#1734,.T.);
#2349=ORIENTED_EDGE('',*,*,#1804,.F.);
#2350=ORIENTED_EDGE('',*,*,#1784,.F.);
#2351=ORIENTED_EDGE('',*,*,#1821,.F.);
#2352=ORIENTED_EDGE('',*,*,#1718,.F.);
#2353=ORIENTED_EDGE('',*,*,#1822,.T.);
#2354=ORIENTED_EDGE('',*,*,#1668,.F.);
#2355=ORIENTED_EDGE('',*,*,#1717,.F.);
#2356=ORIENTED_EDGE('',*,*,#1823,.T.);
#2357=ORIENTED_EDGE('',*,*,#1669,.F.);
#2358=ORIENTED_EDGE('',*,*,#1822,.F.);
#2359=ORIENTED_EDGE('',*,*,#1671,.F.);
#2360=ORIENTED_EDGE('',*,*,#1824,.T.);
#2361=ORIENTED_EDGE('',*,*,#1715,.F.);
#2362=ORIENTED_EDGE('',*,*,#1825,.T.);
#2363=ORIENTED_EDGE('',*,*,#1825,.F.);
#2364=ORIENTED_EDGE('',*,*,#1714,.F.);
#2365=ORIENTED_EDGE('',*,*,#1826,.T.);
#2366=ORIENTED_EDGE('',*,*,#1672,.F.);
#2367=ORIENTED_EDGE('',*,*,#1713,.F.);
#2368=ORIENTED_EDGE('',*,*,#1827,.T.);
#2369=ORIENTED_EDGE('',*,*,#1673,.F.);
#2370=ORIENTED_EDGE('',*,*,#1826,.F.);
#2371=ORIENTED_EDGE('',*,*,#1675,.F.);
#2372=ORIENTED_EDGE('',*,*,#1828,.T.);
#2373=ORIENTED_EDGE('',*,*,#1711,.F.);
#2374=ORIENTED_EDGE('',*,*,#1829,.T.);
#2375=ORIENTED_EDGE('',*,*,#1677,.F.);
#2376=ORIENTED_EDGE('',*,*,#1830,.T.);
#2377=ORIENTED_EDGE('',*,*,#1709,.F.);
#2378=ORIENTED_EDGE('',*,*,#1831,.T.);
#2379=ORIENTED_EDGE('',*,*,#1831,.F.);
#2380=ORIENTED_EDGE('',*,*,#1708,.F.);
#2381=ORIENTED_EDGE('',*,*,#1832,.T.);
#2382=ORIENTED_EDGE('',*,*,#1678,.F.);
#2383=ORIENTED_EDGE('',*,*,#1707,.F.);
#2384=ORIENTED_EDGE('',*,*,#1833,.T.);
#2385=ORIENTED_EDGE('',*,*,#1679,.F.);
#2386=ORIENTED_EDGE('',*,*,#1832,.F.);
#2387=ORIENTED_EDGE('',*,*,#1681,.F.);
#2388=ORIENTED_EDGE('',*,*,#1834,.T.);
#2389=ORIENTED_EDGE('',*,*,#1705,.F.);
#2390=ORIENTED_EDGE('',*,*,#1835,.T.);
#2391=ORIENTED_EDGE('',*,*,#1835,.F.);
#2392=ORIENTED_EDGE('',*,*,#1704,.F.);
#2393=ORIENTED_EDGE('',*,*,#1836,.T.);
#2394=ORIENTED_EDGE('',*,*,#1682,.F.);
#2395=ORIENTED_EDGE('',*,*,#1703,.F.);
#2396=ORIENTED_EDGE('',*,*,#1837,.T.);
#2397=ORIENTED_EDGE('',*,*,#1683,.F.);
#2398=ORIENTED_EDGE('',*,*,#1836,.F.);
#2399=ORIENTED_EDGE('',*,*,#1667,.F.);
#2400=ORIENTED_EDGE('',*,*,#1838,.T.);
#2401=ORIENTED_EDGE('',*,*,#1719,.F.);
#2402=ORIENTED_EDGE('',*,*,#1821,.T.);
#2403=ORIENTED_EDGE('',*,*,#1776,.F.);
#2404=ORIENTED_EDGE('',*,*,#1812,.F.);
#2405=ORIENTED_EDGE('',*,*,#1742,.F.);
#2406=ORIENTED_EDGE('',*,*,#1814,.F.);
#2407=ORIENTED_EDGE('',*,*,#1778,.F.);
#2408=ORIENTED_EDGE('',*,*,#1813,.F.);
#2409=ORIENTED_EDGE('',*,*,#1740,.F.);
#2410=ORIENTED_EDGE('',*,*,#1815,.F.);
#2411=ORIENTED_EDGE('',*,*,#1782,.F.);
#2412=ORIENTED_EDGE('',*,*,#1818,.F.);
#2413=ORIENTED_EDGE('',*,*,#1736,.F.);
#2414=ORIENTED_EDGE('',*,*,#1819,.F.);
#2415=ORIENTED_EDGE('',*,*,#1772,.F.);
#2416=ORIENTED_EDGE('',*,*,#1808,.F.);
#2417=ORIENTED_EDGE('',*,*,#1746,.F.);
#2418=ORIENTED_EDGE('',*,*,#1809,.F.);
#2419=ORIENTED_EDGE('',*,*,#1710,.F.);
#2420=ORIENTED_EDGE('',*,*,#1830,.F.);
#2421=ORIENTED_EDGE('',*,*,#1676,.F.);
#2422=ORIENTED_EDGE('',*,*,#1829,.F.);
#2423=ORIENTED_EDGE('',*,*,#1706,.F.);
#2424=ORIENTED_EDGE('',*,*,#1834,.F.);
#2425=ORIENTED_EDGE('',*,*,#1680,.F.);
#2426=ORIENTED_EDGE('',*,*,#1833,.F.);
#2427=ORIENTED_EDGE('',*,*,#1716,.F.);
#2428=ORIENTED_EDGE('',*,*,#1824,.F.);
#2429=ORIENTED_EDGE('',*,*,#1670,.F.);
#2430=ORIENTED_EDGE('',*,*,#1823,.F.);
#2431=ORIENTED_EDGE('',*,*,#1712,.F.);
#2432=ORIENTED_EDGE('',*,*,#1828,.F.);
#2433=ORIENTED_EDGE('',*,*,#1674,.F.);
#2434=ORIENTED_EDGE('',*,*,#1827,.F.);
#2435=ORIENTED_EDGE('',*,*,#1768,.F.);
#2436=ORIENTED_EDGE('',*,*,#1654,.F.);
#2437=ORIENTED_EDGE('',*,*,#1750,.F.);
#2438=ORIENTED_EDGE('',*,*,#1805,.F.);
#2439=ORIENTED_EDGE('',*,*,#1786,.F.);
#2440=ORIENTED_EDGE('',*,*,#1803,.F.);
#2441=ORIENTED_EDGE('',*,*,#1732,.F.);
#2442=ORIENTED_EDGE('',*,*,#1759,.F.);
#2443=ORIENTED_EDGE('',*,*,#1720,.F.);
#2444=ORIENTED_EDGE('',*,*,#1838,.F.);
#2445=ORIENTED_EDGE('',*,*,#1666,.F.);
#2446=ORIENTED_EDGE('',*,*,#1693,.F.);
#2447=ORIENTED_EDGE('',*,*,#1702,.F.);
#2448=ORIENTED_EDGE('',*,*,#1650,.F.);
#2449=ORIENTED_EDGE('',*,*,#1684,.F.);
#2450=ORIENTED_EDGE('',*,*,#1837,.F.);
#2451=ORIENTED_EDGE('',*,*,#1760,.F.);
#2452=ORIENTED_EDGE('',*,*,#1757,.F.);
#2453=ORIENTED_EDGE('',*,*,#1730,.F.);
#2454=ORIENTED_EDGE('',*,*,#1656,.F.);
#2455=ORIENTED_EDGE('',*,*,#1761,.F.);
#2456=ORIENTED_EDGE('',*,*,#1658,.F.);
#2457=ORIENTED_EDGE('',*,*,#1756,.F.);
#2458=ORIENTED_EDGE('',*,*,#1799,.F.);
#2459=ORIENTED_EDGE('',*,*,#1694,.F.);
#2460=ORIENTED_EDGE('',*,*,#1691,.F.);
#2461=ORIENTED_EDGE('',*,*,#1664,.F.);
#2462=ORIENTED_EDGE('',*,*,#1797,.F.);
#2463=ORIENTED_EDGE('',*,*,#1690,.F.);
#2464=ORIENTED_EDGE('',*,*,#1800,.F.);
#2465=ORIENTED_EDGE('',*,*,#1696,.F.);
#2466=ORIENTED_EDGE('',*,*,#1798,.F.);
#2467=ORIENTED_EDGE('',*,*,#1701,.F.);
#2468=ORIENTED_EDGE('',*,*,#1660,.F.);
#2469=ORIENTED_EDGE('',*,*,#1685,.F.);
#2470=ORIENTED_EDGE('',*,*,#1648,.F.);
#2471=ORIENTED_EDGE('',*,*,#1686,.F.);
#2472=ORIENTED_EDGE('',*,*,#1662,.F.);
#2473=ORIENTED_EDGE('',*,*,#1700,.F.);
#2474=ORIENTED_EDGE('',*,*,#1801,.F.);
#2475=ORIENTED_EDGE('',*,*,#1767,.F.);
#2476=ORIENTED_EDGE('',*,*,#1795,.F.);
#2477=ORIENTED_EDGE('',*,*,#1751,.F.);
#2478=ORIENTED_EDGE('',*,*,#1652,.F.);
#2479=ORIENTED_EDGE('',*,*,#1753,.F.);
#2480=ORIENTED_EDGE('',*,*,#1796,.F.);
#2481=ORIENTED_EDGE('',*,*,#1765,.F.);
#2482=ORIENTED_EDGE('',*,*,#1802,.F.);
#2483=ORIENTED_EDGE('',*,*,#1839,.F.);
#2484=ORIENTED_EDGE('',*,*,#1840,.F.);
#2485=ORIENTED_EDGE('',*,*,#1841,.F.);
#2486=ORIENTED_EDGE('',*,*,#1842,.T.);
#2487=ORIENTED_EDGE('',*,*,#1843,.F.);
#2488=ORIENTED_EDGE('',*,*,#1839,.T.);
#2489=ORIENTED_EDGE('',*,*,#1844,.T.);
#2490=ORIENTED_EDGE('',*,*,#1845,.T.);
#2491=ORIENTED_EDGE('',*,*,#1846,.F.);
#2492=ORIENTED_EDGE('',*,*,#1847,.T.);
#2493=ORIENTED_EDGE('',*,*,#1848,.F.);
#2494=ORIENTED_EDGE('',*,*,#1849,.F.);
#2495=ORIENTED_EDGE('',*,*,#1850,.T.);
#2496=ORIENTED_EDGE('',*,*,#1846,.T.);
#2497=ORIENTED_EDGE('',*,*,#1851,.F.);
#2498=ORIENTED_EDGE('',*,*,#1852,.T.);
#2499=ORIENTED_EDGE('',*,*,#1853,.F.);
#2500=ORIENTED_EDGE('',*,*,#1854,.F.);
#2501=ORIENTED_EDGE('',*,*,#1845,.F.);
#2502=ORIENTED_EDGE('',*,*,#1855,.T.);
#2503=ORIENTED_EDGE('',*,*,#1856,.F.);
#2504=ORIENTED_EDGE('',*,*,#1853,.T.);
#2505=ORIENTED_EDGE('',*,*,#1857,.T.);
#2506=ORIENTED_EDGE('',*,*,#1858,.T.);
#2507=ORIENTED_EDGE('',*,*,#1859,.F.);
#2508=ORIENTED_EDGE('',*,*,#1860,.T.);
#2509=ORIENTED_EDGE('',*,*,#1861,.F.);
#2510=ORIENTED_EDGE('',*,*,#1862,.F.);
#2511=ORIENTED_EDGE('',*,*,#1863,.T.);
#2512=ORIENTED_EDGE('',*,*,#1859,.T.);
#2513=ORIENTED_EDGE('',*,*,#1864,.F.);
#2514=ORIENTED_EDGE('',*,*,#1848,.T.);
#2515=ORIENTED_EDGE('',*,*,#1865,.F.);
#2516=ORIENTED_EDGE('',*,*,#1866,.F.);
#2517=ORIENTED_EDGE('',*,*,#1858,.F.);
#2518=ORIENTED_EDGE('',*,*,#1867,.T.);
#2519=ORIENTED_EDGE('',*,*,#1868,.F.);
#2520=ORIENTED_EDGE('',*,*,#1865,.T.);
#2521=ORIENTED_EDGE('',*,*,#1869,.T.);
#2522=ORIENTED_EDGE('',*,*,#1870,.T.);
#2523=ORIENTED_EDGE('',*,*,#1871,.F.);
#2524=ORIENTED_EDGE('',*,*,#1872,.T.);
#2525=ORIENTED_EDGE('',*,*,#1873,.F.);
#2526=ORIENTED_EDGE('',*,*,#1874,.F.);
#2527=ORIENTED_EDGE('',*,*,#1875,.T.);
#2528=ORIENTED_EDGE('',*,*,#1871,.T.);
#2529=ORIENTED_EDGE('',*,*,#1876,.F.);
#2530=ORIENTED_EDGE('',*,*,#1861,.T.);
#2531=ORIENTED_EDGE('',*,*,#1877,.F.);
#2532=ORIENTED_EDGE('',*,*,#1878,.F.);
#2533=ORIENTED_EDGE('',*,*,#1870,.F.);
#2534=ORIENTED_EDGE('',*,*,#1879,.T.);
#2535=ORIENTED_EDGE('',*,*,#1880,.F.);
#2536=ORIENTED_EDGE('',*,*,#1877,.T.);
#2537=ORIENTED_EDGE('',*,*,#1881,.T.);
#2538=ORIENTED_EDGE('',*,*,#1882,.F.);
#2539=ORIENTED_EDGE('',*,*,#1883,.F.);
#2540=ORIENTED_EDGE('',*,*,#1884,.T.);
#2541=ORIENTED_EDGE('',*,*,#1885,.F.);
#2542=ORIENTED_EDGE('',*,*,#1886,.F.);
#2543=ORIENTED_EDGE('',*,*,#1887,.T.);
#2544=ORIENTED_EDGE('',*,*,#1883,.T.);
#2545=ORIENTED_EDGE('',*,*,#1888,.F.);
#2546=ORIENTED_EDGE('',*,*,#1873,.T.);
#2547=ORIENTED_EDGE('',*,*,#1889,.T.);
#2548=ORIENTED_EDGE('',*,*,#1890,.F.);
#2549=ORIENTED_EDGE('',*,*,#1881,.F.);
#2550=ORIENTED_EDGE('',*,*,#1891,.T.);
#2551=ORIENTED_EDGE('',*,*,#1892,.F.);
#2552=ORIENTED_EDGE('',*,*,#1893,.F.);
#2553=ORIENTED_EDGE('',*,*,#1882,.T.);
#2554=ORIENTED_EDGE('',*,*,#1890,.T.);
#2555=ORIENTED_EDGE('',*,*,#1894,.F.);
#2556=ORIENTED_EDGE('',*,*,#1895,.F.);
#2557=ORIENTED_EDGE('',*,*,#1880,.T.);
#2558=ORIENTED_EDGE('',*,*,#1893,.T.);
#2559=ORIENTED_EDGE('',*,*,#1884,.F.);
#2560=ORIENTED_EDGE('',*,*,#1896,.F.);
#2561=ORIENTED_EDGE('',*,*,#1878,.T.);
#2562=ORIENTED_EDGE('',*,*,#1895,.T.);
#2563=ORIENTED_EDGE('',*,*,#1887,.F.);
#2564=ORIENTED_EDGE('',*,*,#1897,.F.);
#2565=ORIENTED_EDGE('',*,*,#1868,.T.);
#2566=ORIENTED_EDGE('',*,*,#1896,.T.);
#2567=ORIENTED_EDGE('',*,*,#1872,.F.);
#2568=ORIENTED_EDGE('',*,*,#1898,.F.);
#2569=ORIENTED_EDGE('',*,*,#1866,.T.);
#2570=ORIENTED_EDGE('',*,*,#1897,.T.);
#2571=ORIENTED_EDGE('',*,*,#1875,.F.);
#2572=ORIENTED_EDGE('',*,*,#1899,.F.);
#2573=ORIENTED_EDGE('',*,*,#1856,.T.);
#2574=ORIENTED_EDGE('',*,*,#1898,.T.);
#2575=ORIENTED_EDGE('',*,*,#1860,.F.);
#2576=ORIENTED_EDGE('',*,*,#1900,.F.);
#2577=ORIENTED_EDGE('',*,*,#1854,.T.);
#2578=ORIENTED_EDGE('',*,*,#1899,.T.);
#2579=ORIENTED_EDGE('',*,*,#1863,.F.);
#2580=ORIENTED_EDGE('',*,*,#1901,.F.);
#2581=ORIENTED_EDGE('',*,*,#1843,.T.);
#2582=ORIENTED_EDGE('',*,*,#1900,.T.);
#2583=ORIENTED_EDGE('',*,*,#1847,.F.);
#2584=ORIENTED_EDGE('',*,*,#1902,.F.);
#2585=ORIENTED_EDGE('',*,*,#1840,.T.);
#2586=ORIENTED_EDGE('',*,*,#1901,.T.);
#2587=ORIENTED_EDGE('',*,*,#1850,.F.);
#2588=ORIENTED_EDGE('',*,*,#1903,.F.);
#2589=ORIENTED_EDGE('',*,*,#1904,.T.);
#2590=ORIENTED_EDGE('',*,*,#1902,.T.);
#2591=ORIENTED_EDGE('',*,*,#1852,.F.);
#2592=ORIENTED_EDGE('',*,*,#1905,.F.);
#2593=ORIENTED_EDGE('',*,*,#1906,.T.);
#2594=ORIENTED_EDGE('',*,*,#1903,.T.);
#2595=ORIENTED_EDGE('',*,*,#1851,.T.);
#2596=ORIENTED_EDGE('',*,*,#1907,.F.);
#2597=ORIENTED_EDGE('',*,*,#1908,.F.);
#2598=ORIENTED_EDGE('',*,*,#1905,.T.);
#2599=ORIENTED_EDGE('',*,*,#1849,.T.);
#2600=ORIENTED_EDGE('',*,*,#1909,.F.);
#2601=ORIENTED_EDGE('',*,*,#1842,.F.);
#2602=ORIENTED_EDGE('',*,*,#1907,.T.);
#2603=ORIENTED_EDGE('',*,*,#1864,.T.);
#2604=ORIENTED_EDGE('',*,*,#1910,.F.);
#2605=ORIENTED_EDGE('',*,*,#1844,.F.);
#2606=ORIENTED_EDGE('',*,*,#1909,.T.);
#2607=ORIENTED_EDGE('',*,*,#1862,.T.);
#2608=ORIENTED_EDGE('',*,*,#1911,.F.);
#2609=ORIENTED_EDGE('',*,*,#1855,.F.);
#2610=ORIENTED_EDGE('',*,*,#1910,.T.);
#2611=ORIENTED_EDGE('',*,*,#1876,.T.);
#2612=ORIENTED_EDGE('',*,*,#1912,.F.);
#2613=ORIENTED_EDGE('',*,*,#1857,.F.);
#2614=ORIENTED_EDGE('',*,*,#1911,.T.);
#2615=ORIENTED_EDGE('',*,*,#1874,.T.);
#2616=ORIENTED_EDGE('',*,*,#1913,.F.);
#2617=ORIENTED_EDGE('',*,*,#1867,.F.);
#2618=ORIENTED_EDGE('',*,*,#1912,.T.);
#2619=ORIENTED_EDGE('',*,*,#1888,.T.);
#2620=ORIENTED_EDGE('',*,*,#1914,.F.);
#2621=ORIENTED_EDGE('',*,*,#1869,.F.);
#2622=ORIENTED_EDGE('',*,*,#1913,.T.);
#2623=ORIENTED_EDGE('',*,*,#1886,.T.);
#2624=ORIENTED_EDGE('',*,*,#1891,.F.);
#2625=ORIENTED_EDGE('',*,*,#1879,.F.);
#2626=ORIENTED_EDGE('',*,*,#1914,.T.);
#2627=ORIENTED_EDGE('',*,*,#1908,.T.);
#2628=ORIENTED_EDGE('',*,*,#1841,.T.);
#2629=ORIENTED_EDGE('',*,*,#1904,.F.);
#2630=ORIENTED_EDGE('',*,*,#1906,.F.);
#2631=ORIENTED_EDGE('',*,*,#1889,.F.);
#2632=ORIENTED_EDGE('',*,*,#1885,.T.);
#2633=ORIENTED_EDGE('',*,*,#1894,.T.);
#2634=ORIENTED_EDGE('',*,*,#1892,.T.);
#2635=ORIENTED_EDGE('',*,*,#1915,.T.);
#2636=ORIENTED_EDGE('',*,*,#1916,.F.);
#2637=ORIENTED_EDGE('',*,*,#1917,.F.);
#2638=ORIENTED_EDGE('',*,*,#1918,.T.);
#2639=ORIENTED_EDGE('',*,*,#1919,.T.);
#2640=ORIENTED_EDGE('',*,*,#1920,.F.);
#2641=ORIENTED_EDGE('',*,*,#1921,.F.);
#2642=ORIENTED_EDGE('',*,*,#1916,.T.);
#2643=ORIENTED_EDGE('',*,*,#1922,.T.);
#2644=ORIENTED_EDGE('',*,*,#1923,.T.);
#2645=ORIENTED_EDGE('',*,*,#1924,.T.);
#2646=ORIENTED_EDGE('',*,*,#1925,.T.);
#2647=ORIENTED_EDGE('',*,*,#1926,.T.);
#2648=ORIENTED_EDGE('',*,*,#1927,.T.);
#2649=ORIENTED_EDGE('',*,*,#1928,.T.);
#2650=ORIENTED_EDGE('',*,*,#1929,.T.);
#2651=ORIENTED_EDGE('',*,*,#1930,.T.);
#2652=ORIENTED_EDGE('',*,*,#1931,.F.);
#2653=ORIENTED_EDGE('',*,*,#1932,.F.);
#2654=ORIENTED_EDGE('',*,*,#1920,.T.);
#2655=ORIENTED_EDGE('',*,*,#1933,.T.);
#2656=ORIENTED_EDGE('',*,*,#1934,.F.);
#2657=ORIENTED_EDGE('',*,*,#1935,.F.);
#2658=ORIENTED_EDGE('',*,*,#1931,.T.);
#2659=ORIENTED_EDGE('',*,*,#1936,.T.);
#2660=ORIENTED_EDGE('',*,*,#1937,.F.);
#2661=ORIENTED_EDGE('',*,*,#1938,.F.);
#2662=ORIENTED_EDGE('',*,*,#1934,.T.);
#2663=ORIENTED_EDGE('',*,*,#1939,.T.);
#2664=ORIENTED_EDGE('',*,*,#1940,.F.);
#2665=ORIENTED_EDGE('',*,*,#1941,.F.);
#2666=ORIENTED_EDGE('',*,*,#1937,.T.);
#2667=ORIENTED_EDGE('',*,*,#1942,.T.);
#2668=ORIENTED_EDGE('',*,*,#1943,.F.);
#2669=ORIENTED_EDGE('',*,*,#1944,.F.);
#2670=ORIENTED_EDGE('',*,*,#1940,.T.);
#2671=ORIENTED_EDGE('',*,*,#1945,.F.);
#2672=ORIENTED_EDGE('',*,*,#1946,.F.);
#2673=ORIENTED_EDGE('',*,*,#1947,.F.);
#2674=ORIENTED_EDGE('',*,*,#1948,.F.);
#2675=ORIENTED_EDGE('',*,*,#1949,.F.);
#2676=ORIENTED_EDGE('',*,*,#1950,.F.);
#2677=ORIENTED_EDGE('',*,*,#1951,.F.);
#2678=ORIENTED_EDGE('',*,*,#1952,.F.);
#2679=ORIENTED_EDGE('',*,*,#1953,.T.);
#2680=ORIENTED_EDGE('',*,*,#1918,.F.);
#2681=ORIENTED_EDGE('',*,*,#1954,.F.);
#2682=ORIENTED_EDGE('',*,*,#1943,.T.);
#2683=ORIENTED_EDGE('',*,*,#1917,.T.);
#2684=ORIENTED_EDGE('',*,*,#1921,.T.);
#2685=ORIENTED_EDGE('',*,*,#1932,.T.);
#2686=ORIENTED_EDGE('',*,*,#1935,.T.);
#2687=ORIENTED_EDGE('',*,*,#1938,.T.);
#2688=ORIENTED_EDGE('',*,*,#1941,.T.);
#2689=ORIENTED_EDGE('',*,*,#1944,.T.);
#2690=ORIENTED_EDGE('',*,*,#1954,.T.);
#2691=ORIENTED_EDGE('',*,*,#1915,.F.);
#2692=ORIENTED_EDGE('',*,*,#1953,.F.);
#2693=ORIENTED_EDGE('',*,*,#1942,.F.);
#2694=ORIENTED_EDGE('',*,*,#1939,.F.);
#2695=ORIENTED_EDGE('',*,*,#1936,.F.);
#2696=ORIENTED_EDGE('',*,*,#1933,.F.);
#2697=ORIENTED_EDGE('',*,*,#1930,.F.);
#2698=ORIENTED_EDGE('',*,*,#1919,.F.);
#2699=ORIENTED_EDGE('',*,*,#1955,.T.);
#2700=ORIENTED_EDGE('',*,*,#1950,.T.);
#2701=ORIENTED_EDGE('',*,*,#1956,.F.);
#2702=ORIENTED_EDGE('',*,*,#1927,.F.);
#2703=ORIENTED_EDGE('',*,*,#1957,.T.);
#2704=ORIENTED_EDGE('',*,*,#1951,.T.);
#2705=ORIENTED_EDGE('',*,*,#1955,.F.);
#2706=ORIENTED_EDGE('',*,*,#1926,.F.);
#2707=ORIENTED_EDGE('',*,*,#1958,.T.);
#2708=ORIENTED_EDGE('',*,*,#1952,.T.);
#2709=ORIENTED_EDGE('',*,*,#1957,.F.);
#2710=ORIENTED_EDGE('',*,*,#1929,.F.);
#2711=ORIENTED_EDGE('',*,*,#1956,.T.);
#2712=ORIENTED_EDGE('',*,*,#1949,.T.);
#2713=ORIENTED_EDGE('',*,*,#1958,.F.);
#2714=ORIENTED_EDGE('',*,*,#1928,.F.);
#2715=ORIENTED_EDGE('',*,*,#1959,.T.);
#2716=ORIENTED_EDGE('',*,*,#1946,.T.);
#2717=ORIENTED_EDGE('',*,*,#1960,.F.);
#2718=ORIENTED_EDGE('',*,*,#1923,.F.);
#2719=ORIENTED_EDGE('',*,*,#1961,.T.);
#2720=ORIENTED_EDGE('',*,*,#1947,.T.);
#2721=ORIENTED_EDGE('',*,*,#1959,.F.);
#2722=ORIENTED_EDGE('',*,*,#1922,.F.);
#2723=ORIENTED_EDGE('',*,*,#1962,.T.);
#2724=ORIENTED_EDGE('',*,*,#1948,.T.);
#2725=ORIENTED_EDGE('',*,*,#1961,.F.);
#2726=ORIENTED_EDGE('',*,*,#1925,.F.);
#2727=ORIENTED_EDGE('',*,*,#1960,.T.);
#2728=ORIENTED_EDGE('',*,*,#1945,.T.);
#2729=ORIENTED_EDGE('',*,*,#1962,.F.);
#2730=ORIENTED_EDGE('',*,*,#1924,.F.);
#2731=ORIENTED_EDGE('',*,*,#1963,.F.);
#2732=ORIENTED_EDGE('',*,*,#1964,.F.);
#2733=ORIENTED_EDGE('',*,*,#1965,.F.);
#2734=ORIENTED_EDGE('',*,*,#1966,.T.);
#2735=ORIENTED_EDGE('',*,*,#1967,.F.);
#2736=ORIENTED_EDGE('',*,*,#1963,.T.);
#2737=ORIENTED_EDGE('',*,*,#1968,.T.);
#2738=ORIENTED_EDGE('',*,*,#1969,.F.);
#2739=ORIENTED_EDGE('',*,*,#1970,.F.);
#2740=ORIENTED_EDGE('',*,*,#1971,.T.);
#2741=ORIENTED_EDGE('',*,*,#1972,.F.);
#2742=ORIENTED_EDGE('',*,*,#1973,.F.);
#2743=ORIENTED_EDGE('',*,*,#1974,.T.);
#2744=ORIENTED_EDGE('',*,*,#1970,.T.);
#2745=ORIENTED_EDGE('',*,*,#1975,.F.);
#2746=ORIENTED_EDGE('',*,*,#1976,.T.);
#2747=ORIENTED_EDGE('',*,*,#1977,.T.);
#2748=ORIENTED_EDGE('',*,*,#1978,.F.);
#2749=ORIENTED_EDGE('',*,*,#1968,.F.);
#2750=ORIENTED_EDGE('',*,*,#1979,.T.);
#2751=ORIENTED_EDGE('',*,*,#1980,.T.);
#2752=ORIENTED_EDGE('',*,*,#1981,.T.);
#2753=ORIENTED_EDGE('',*,*,#1982,.T.);
#2754=ORIENTED_EDGE('',*,*,#1983,.T.);
#2755=ORIENTED_EDGE('',*,*,#1984,.T.);
#2756=ORIENTED_EDGE('',*,*,#1985,.T.);
#2757=ORIENTED_EDGE('',*,*,#1986,.T.);
#2758=ORIENTED_EDGE('',*,*,#1987,.T.);
#2759=ORIENTED_EDGE('',*,*,#1988,.F.);
#2760=ORIENTED_EDGE('',*,*,#1989,.F.);
#2761=ORIENTED_EDGE('',*,*,#1969,.T.);
#2762=ORIENTED_EDGE('',*,*,#1978,.T.);
#2763=ORIENTED_EDGE('',*,*,#1990,.F.);
#2764=ORIENTED_EDGE('',*,*,#1991,.F.);
#2765=ORIENTED_EDGE('',*,*,#1967,.T.);
#2766=ORIENTED_EDGE('',*,*,#1989,.T.);
#2767=ORIENTED_EDGE('',*,*,#1992,.F.);
#2768=ORIENTED_EDGE('',*,*,#1993,.F.);
#2769=ORIENTED_EDGE('',*,*,#1994,.F.);
#2770=ORIENTED_EDGE('',*,*,#1995,.F.);
#2771=ORIENTED_EDGE('',*,*,#1996,.F.);
#2772=ORIENTED_EDGE('',*,*,#1997,.F.);
#2773=ORIENTED_EDGE('',*,*,#1998,.F.);
#2774=ORIENTED_EDGE('',*,*,#1999,.F.);
#2775=ORIENTED_EDGE('',*,*,#1971,.F.);
#2776=ORIENTED_EDGE('',*,*,#2000,.F.);
#2777=ORIENTED_EDGE('',*,*,#1964,.T.);
#2778=ORIENTED_EDGE('',*,*,#1991,.T.);
#2779=ORIENTED_EDGE('',*,*,#1974,.F.);
#2780=ORIENTED_EDGE('',*,*,#2001,.F.);
#2781=ORIENTED_EDGE('',*,*,#2002,.T.);
#2782=ORIENTED_EDGE('',*,*,#2000,.T.);
#2783=ORIENTED_EDGE('',*,*,#1976,.F.);
#2784=ORIENTED_EDGE('',*,*,#2003,.F.);
#2785=ORIENTED_EDGE('',*,*,#2004,.T.);
#2786=ORIENTED_EDGE('',*,*,#2001,.T.);
#2787=ORIENTED_EDGE('',*,*,#1975,.T.);
#2788=ORIENTED_EDGE('',*,*,#2005,.F.);
#2789=ORIENTED_EDGE('',*,*,#2006,.F.);
#2790=ORIENTED_EDGE('',*,*,#2003,.T.);
#2791=ORIENTED_EDGE('',*,*,#1973,.T.);
#2792=ORIENTED_EDGE('',*,*,#1979,.F.);
#2793=ORIENTED_EDGE('',*,*,#1966,.F.);
#2794=ORIENTED_EDGE('',*,*,#2005,.T.);
#2795=ORIENTED_EDGE('',*,*,#2006,.T.);
#2796=ORIENTED_EDGE('',*,*,#1965,.T.);
#2797=ORIENTED_EDGE('',*,*,#2002,.F.);
#2798=ORIENTED_EDGE('',*,*,#2004,.F.);
#2799=ORIENTED_EDGE('',*,*,#1977,.F.);
#2800=ORIENTED_EDGE('',*,*,#1972,.T.);
#2801=ORIENTED_EDGE('',*,*,#1990,.T.);
#2802=ORIENTED_EDGE('',*,*,#1988,.T.);
#2803=ORIENTED_EDGE('',*,*,#2007,.T.);
#2804=ORIENTED_EDGE('',*,*,#1996,.T.);
#2805=ORIENTED_EDGE('',*,*,#2008,.F.);
#2806=ORIENTED_EDGE('',*,*,#1985,.F.);
#2807=ORIENTED_EDGE('',*,*,#2009,.T.);
#2808=ORIENTED_EDGE('',*,*,#1997,.T.);
#2809=ORIENTED_EDGE('',*,*,#2007,.F.);
#2810=ORIENTED_EDGE('',*,*,#1984,.F.);
#2811=ORIENTED_EDGE('',*,*,#2010,.T.);
#2812=ORIENTED_EDGE('',*,*,#1998,.T.);
#2813=ORIENTED_EDGE('',*,*,#2009,.F.);
#2814=ORIENTED_EDGE('',*,*,#1987,.F.);
#2815=ORIENTED_EDGE('',*,*,#2008,.T.);
#2816=ORIENTED_EDGE('',*,*,#1999,.T.);
#2817=ORIENTED_EDGE('',*,*,#2010,.F.);
#2818=ORIENTED_EDGE('',*,*,#1986,.F.);
#2819=ORIENTED_EDGE('',*,*,#2011,.T.);
#2820=ORIENTED_EDGE('',*,*,#1992,.T.);
#2821=ORIENTED_EDGE('',*,*,#2012,.F.);
#2822=ORIENTED_EDGE('',*,*,#1981,.F.);
#2823=ORIENTED_EDGE('',*,*,#2013,.T.);
#2824=ORIENTED_EDGE('',*,*,#1993,.T.);
#2825=ORIENTED_EDGE('',*,*,#2011,.F.);
#2826=ORIENTED_EDGE('',*,*,#1980,.F.);
#2827=ORIENTED_EDGE('',*,*,#2014,.T.);
#2828=ORIENTED_EDGE('',*,*,#1994,.T.);
#2829=ORIENTED_EDGE('',*,*,#2013,.F.);
#2830=ORIENTED_EDGE('',*,*,#1983,.F.);
#2831=ORIENTED_EDGE('',*,*,#2012,.T.);
#2832=ORIENTED_EDGE('',*,*,#1995,.T.);
#2833=ORIENTED_EDGE('',*,*,#2014,.F.);
#2834=ORIENTED_EDGE('',*,*,#1982,.F.);
#2835=ORIENTED_EDGE('',*,*,#2015,.F.);
#2836=ORIENTED_EDGE('',*,*,#2016,.T.);
#2837=ORIENTED_EDGE('',*,*,#2017,.F.);
#2838=ORIENTED_EDGE('',*,*,#2016,.F.);
#2839=ORIENTED_EDGE('',*,*,#2018,.F.);
#2840=ORIENTED_EDGE('',*,*,#2019,.T.);
#2841=ORIENTED_EDGE('',*,*,#2020,.T.);
#2842=ORIENTED_EDGE('',*,*,#2019,.F.);
#2843=ORIENTED_EDGE('',*,*,#2021,.F.);
#2844=ORIENTED_EDGE('',*,*,#2022,.T.);
#2845=ORIENTED_EDGE('',*,*,#2023,.T.);
#2846=ORIENTED_EDGE('',*,*,#2022,.F.);
#2847=ORIENTED_EDGE('',*,*,#2024,.T.);
#2848=ORIENTED_EDGE('',*,*,#2025,.F.);
#2849=ORIENTED_EDGE('',*,*,#2026,.F.);
#2850=ORIENTED_EDGE('',*,*,#2027,.T.);
#2851=ORIENTED_EDGE('',*,*,#2028,.T.);
#2852=ORIENTED_EDGE('',*,*,#2029,.F.);
#2853=ORIENTED_EDGE('',*,*,#2030,.F.);
#2854=ORIENTED_EDGE('',*,*,#2025,.T.);
#2855=ORIENTED_EDGE('',*,*,#2018,.T.);
#2856=ORIENTED_EDGE('',*,*,#2031,.T.);
#2857=ORIENTED_EDGE('',*,*,#2032,.F.);
#2858=ORIENTED_EDGE('',*,*,#2033,.F.);
#2859=ORIENTED_EDGE('',*,*,#2029,.T.);
#2860=ORIENTED_EDGE('',*,*,#2034,.T.);
#2861=ORIENTED_EDGE('',*,*,#2035,.F.);
#2862=ORIENTED_EDGE('',*,*,#2036,.F.);
#2863=ORIENTED_EDGE('',*,*,#2032,.T.);
#2864=ORIENTED_EDGE('',*,*,#2037,.T.);
#2865=ORIENTED_EDGE('',*,*,#2038,.F.);
#2866=ORIENTED_EDGE('',*,*,#2039,.F.);
#2867=ORIENTED_EDGE('',*,*,#2035,.T.);
#2868=ORIENTED_EDGE('',*,*,#2040,.T.);
#2869=ORIENTED_EDGE('',*,*,#2041,.F.);
#2870=ORIENTED_EDGE('',*,*,#2042,.F.);
#2871=ORIENTED_EDGE('',*,*,#2038,.T.);
#2872=ORIENTED_EDGE('',*,*,#2017,.T.);
#2873=ORIENTED_EDGE('',*,*,#2043,.T.);
#2874=ORIENTED_EDGE('',*,*,#2044,.F.);
#2875=ORIENTED_EDGE('',*,*,#2045,.F.);
#2876=ORIENTED_EDGE('',*,*,#2041,.T.);
#2877=ORIENTED_EDGE('',*,*,#2046,.T.);
#2878=ORIENTED_EDGE('',*,*,#2047,.F.);
#2879=ORIENTED_EDGE('',*,*,#2048,.F.);
#2880=ORIENTED_EDGE('',*,*,#2044,.T.);
#2881=ORIENTED_EDGE('',*,*,#2049,.T.);
#2882=ORIENTED_EDGE('',*,*,#2050,.F.);
#2883=ORIENTED_EDGE('',*,*,#2051,.F.);
#2884=ORIENTED_EDGE('',*,*,#2047,.T.);
#2885=ORIENTED_EDGE('',*,*,#2052,.T.);
#2886=ORIENTED_EDGE('',*,*,#2053,.F.);
#2887=ORIENTED_EDGE('',*,*,#2054,.F.);
#2888=ORIENTED_EDGE('',*,*,#2050,.T.);
#2889=ORIENTED_EDGE('',*,*,#2015,.T.);
#2890=ORIENTED_EDGE('',*,*,#2055,.T.);
#2891=ORIENTED_EDGE('',*,*,#2056,.F.);
#2892=ORIENTED_EDGE('',*,*,#2057,.F.);
#2893=ORIENTED_EDGE('',*,*,#2053,.T.);
#2894=ORIENTED_EDGE('',*,*,#2058,.T.);
#2895=ORIENTED_EDGE('',*,*,#2059,.F.);
#2896=ORIENTED_EDGE('',*,*,#2060,.F.);
#2897=ORIENTED_EDGE('',*,*,#2056,.T.);
#2898=ORIENTED_EDGE('',*,*,#2061,.T.);
#2899=ORIENTED_EDGE('',*,*,#2062,.F.);
#2900=ORIENTED_EDGE('',*,*,#2063,.F.);
#2901=ORIENTED_EDGE('',*,*,#2059,.T.);
#2902=ORIENTED_EDGE('',*,*,#2064,.T.);
#2903=ORIENTED_EDGE('',*,*,#2065,.F.);
#2904=ORIENTED_EDGE('',*,*,#2066,.F.);
#2905=ORIENTED_EDGE('',*,*,#2062,.T.);
#2906=ORIENTED_EDGE('',*,*,#2021,.T.);
#2907=ORIENTED_EDGE('',*,*,#2067,.T.);
#2908=ORIENTED_EDGE('',*,*,#2068,.F.);
#2909=ORIENTED_EDGE('',*,*,#2069,.F.);
#2910=ORIENTED_EDGE('',*,*,#2065,.T.);
#2911=ORIENTED_EDGE('',*,*,#2070,.T.);
#2912=ORIENTED_EDGE('',*,*,#2071,.F.);
#2913=ORIENTED_EDGE('',*,*,#2072,.F.);
#2914=ORIENTED_EDGE('',*,*,#2068,.T.);
#2915=ORIENTED_EDGE('',*,*,#2073,.T.);
#2916=ORIENTED_EDGE('',*,*,#2074,.F.);
#2917=ORIENTED_EDGE('',*,*,#2075,.F.);
#2918=ORIENTED_EDGE('',*,*,#2071,.T.);
#2919=ORIENTED_EDGE('',*,*,#2076,.T.);
#2920=ORIENTED_EDGE('',*,*,#2077,.F.);
#2921=ORIENTED_EDGE('',*,*,#2078,.F.);
#2922=ORIENTED_EDGE('',*,*,#2074,.T.);
#2923=ORIENTED_EDGE('',*,*,#2023,.F.);
#2924=ORIENTED_EDGE('',*,*,#2079,.T.);
#2925=ORIENTED_EDGE('',*,*,#2080,.F.);
#2926=ORIENTED_EDGE('',*,*,#2081,.F.);
#2927=ORIENTED_EDGE('',*,*,#2077,.T.);
#2928=ORIENTED_EDGE('',*,*,#2082,.T.);
#2929=ORIENTED_EDGE('',*,*,#2083,.F.);
#2930=ORIENTED_EDGE('',*,*,#2084,.F.);
#2931=ORIENTED_EDGE('',*,*,#2080,.T.);
#2932=ORIENTED_EDGE('',*,*,#2085,.T.);
#2933=ORIENTED_EDGE('',*,*,#2086,.F.);
#2934=ORIENTED_EDGE('',*,*,#2087,.F.);
#2935=ORIENTED_EDGE('',*,*,#2083,.T.);
#2936=ORIENTED_EDGE('',*,*,#2088,.T.);
#2937=ORIENTED_EDGE('',*,*,#2089,.F.);
#2938=ORIENTED_EDGE('',*,*,#2090,.F.);
#2939=ORIENTED_EDGE('',*,*,#2086,.T.);
#2940=ORIENTED_EDGE('',*,*,#2020,.F.);
#2941=ORIENTED_EDGE('',*,*,#2091,.T.);
#2942=ORIENTED_EDGE('',*,*,#2092,.F.);
#2943=ORIENTED_EDGE('',*,*,#2093,.F.);
#2944=ORIENTED_EDGE('',*,*,#2089,.T.);
#2945=ORIENTED_EDGE('',*,*,#2094,.T.);
#2946=ORIENTED_EDGE('',*,*,#2027,.F.);
#2947=ORIENTED_EDGE('',*,*,#2095,.F.);
#2948=ORIENTED_EDGE('',*,*,#2092,.T.);
#2949=ORIENTED_EDGE('',*,*,#2026,.T.);
#2950=ORIENTED_EDGE('',*,*,#2030,.T.);
#2951=ORIENTED_EDGE('',*,*,#2033,.T.);
#2952=ORIENTED_EDGE('',*,*,#2036,.T.);
#2953=ORIENTED_EDGE('',*,*,#2039,.T.);
#2954=ORIENTED_EDGE('',*,*,#2042,.T.);
#2955=ORIENTED_EDGE('',*,*,#2045,.T.);
#2956=ORIENTED_EDGE('',*,*,#2048,.T.);
#2957=ORIENTED_EDGE('',*,*,#2051,.T.);
#2958=ORIENTED_EDGE('',*,*,#2054,.T.);
#2959=ORIENTED_EDGE('',*,*,#2057,.T.);
#2960=ORIENTED_EDGE('',*,*,#2060,.T.);
#2961=ORIENTED_EDGE('',*,*,#2063,.T.);
#2962=ORIENTED_EDGE('',*,*,#2066,.T.);
#2963=ORIENTED_EDGE('',*,*,#2069,.T.);
#2964=ORIENTED_EDGE('',*,*,#2072,.T.);
#2965=ORIENTED_EDGE('',*,*,#2075,.T.);
#2966=ORIENTED_EDGE('',*,*,#2078,.T.);
#2967=ORIENTED_EDGE('',*,*,#2081,.T.);
#2968=ORIENTED_EDGE('',*,*,#2084,.T.);
#2969=ORIENTED_EDGE('',*,*,#2087,.T.);
#2970=ORIENTED_EDGE('',*,*,#2090,.T.);
#2971=ORIENTED_EDGE('',*,*,#2093,.T.);
#2972=ORIENTED_EDGE('',*,*,#2095,.T.);
#2973=ORIENTED_EDGE('',*,*,#2024,.F.);
#2974=ORIENTED_EDGE('',*,*,#2094,.F.);
#2975=ORIENTED_EDGE('',*,*,#2091,.F.);
#2976=ORIENTED_EDGE('',*,*,#2088,.F.);
#2977=ORIENTED_EDGE('',*,*,#2085,.F.);
#2978=ORIENTED_EDGE('',*,*,#2082,.F.);
#2979=ORIENTED_EDGE('',*,*,#2079,.F.);
#2980=ORIENTED_EDGE('',*,*,#2076,.F.);
#2981=ORIENTED_EDGE('',*,*,#2073,.F.);
#2982=ORIENTED_EDGE('',*,*,#2070,.F.);
#2983=ORIENTED_EDGE('',*,*,#2067,.F.);
#2984=ORIENTED_EDGE('',*,*,#2064,.F.);
#2985=ORIENTED_EDGE('',*,*,#2061,.F.);
#2986=ORIENTED_EDGE('',*,*,#2058,.F.);
#2987=ORIENTED_EDGE('',*,*,#2055,.F.);
#2988=ORIENTED_EDGE('',*,*,#2052,.F.);
#2989=ORIENTED_EDGE('',*,*,#2049,.F.);
#2990=ORIENTED_EDGE('',*,*,#2046,.F.);
#2991=ORIENTED_EDGE('',*,*,#2043,.F.);
#2992=ORIENTED_EDGE('',*,*,#2040,.F.);
#2993=ORIENTED_EDGE('',*,*,#2037,.F.);
#2994=ORIENTED_EDGE('',*,*,#2034,.F.);
#2995=ORIENTED_EDGE('',*,*,#2031,.F.);
#2996=ORIENTED_EDGE('',*,*,#2028,.F.);
#2997=ORIENTED_EDGE('',*,*,#2096,.T.);
#2998=ORIENTED_EDGE('',*,*,#2097,.T.);
#2999=ORIENTED_EDGE('',*,*,#2098,.F.);
#3000=ORIENTED_EDGE('',*,*,#2097,.F.);
#3001=ORIENTED_EDGE('',*,*,#2098,.T.);
#3002=ORIENTED_EDGE('',*,*,#2096,.F.);
#3003=PLANE('',#3382);
#3004=PLANE('',#3383);
#3005=PLANE('',#3384);
#3006=PLANE('',#3385);
#3007=PLANE('',#3386);
#3008=PLANE('',#3391);
#3009=PLANE('',#3392);
#3010=PLANE('',#3400);
#3011=PLANE('',#3404);
#3012=PLANE('',#3409);
#3013=PLANE('',#3410);
#3014=PLANE('',#3418);
#3015=PLANE('',#3422);
#3016=PLANE('',#3423);
#3017=PLANE('',#3424);
#3018=PLANE('',#3425);
#3019=PLANE('',#3426);
#3020=PLANE('',#3427);
#3021=PLANE('',#3428);
#3022=PLANE('',#3429);
#3023=PLANE('',#3430);
#3024=PLANE('',#3431);
#3025=PLANE('',#3432);
#3026=PLANE('',#3433);
#3027=PLANE('',#3434);
#3028=PLANE('',#3435);
#3029=PLANE('',#3436);
#3030=PLANE('',#3437);
#3031=PLANE('',#3438);
#3032=PLANE('',#3439);
#3033=PLANE('',#3440);
#3034=PLANE('',#3441);
#3035=PLANE('',#3442);
#3036=PLANE('',#3443);
#3037=PLANE('',#3444);
#3038=PLANE('',#3445);
#3039=PLANE('',#3446);
#3040=PLANE('',#3447);
#3041=PLANE('',#3448);
#3042=PLANE('',#3449);
#3043=PLANE('',#3450);
#3044=PLANE('',#3451);
#3045=PLANE('',#3452);
#3046=PLANE('',#3453);
#3047=PLANE('',#3454);
#3048=PLANE('',#3455);
#3049=PLANE('',#3456);
#3050=PLANE('',#3457);
#3051=PLANE('',#3458);
#3052=PLANE('',#3459);
#3053=PLANE('',#3460);
#3054=PLANE('',#3461);
#3055=PLANE('',#3462);
#3056=PLANE('',#3463);
#3057=PLANE('',#3473);
#3058=PLANE('',#3476);
#3059=PLANE('',#3477);
#3060=PLANE('',#3480);
#3061=PLANE('',#3481);
#3062=PLANE('',#3484);
#3063=PLANE('',#3485);
#3064=PLANE('',#3488);
#3065=PLANE('',#3489);
#3066=PLANE('',#3492);
#3067=PLANE('',#3493);
#3068=PLANE('',#3496);
#3069=PLANE('',#3497);
#3070=PLANE('',#3500);
#3071=PLANE('',#3501);
#3072=PLANE('',#3504);
#3073=PLANE('',#3505);
#3074=PLANE('',#3506);
#3075=PLANE('',#3507);
#3076=PLANE('',#3509);
#3077=PLANE('',#3511);
#3078=PLANE('',#3513);
#3079=PLANE('',#3515);
#3080=PLANE('',#3516);
#3081=PLANE('',#3517);
#3082=PLANE('',#3519);
#3083=PLANE('',#3521);
#3084=PLANE('',#3523);
#3085=PLANE('',#3525);
#3086=PLANE('',#3526);
#3087=PLANE('',#3528);
#3088=PLANE('',#3529);
#3089=PLANE('',#3534);
#3090=PLANE('',#3535);
#3091=PLANE('',#3539);
#3092=PLANE('',#3540);
#3093=PLANE('',#3548);
#3094=PLANE('',#3549);
#3095=PLANE('',#3551);
#3096=PLANE('',#3553);
#3097=PLANE('',#3555);
#3098=PLANE('',#3557);
#3099=PLANE('',#3559);
#3100=PLANE('',#3562);
#3101=PLANE('',#3563);
#3102=PLANE('',#3566);
#3103=PLANE('',#3567);
#3104=PLANE('',#3572);
#3105=PLANE('',#3573);
#3106=PLANE('',#3579);
#3107=PLANE('',#3580);
#3108=PLANE('',#3581);
#3109=PLANE('',#3583);
#3110=PLANE('',#3584);
#3111=PLANE('',#3586);
#3112=PLANE('',#3588);
#3113=PLANE('',#3590);
#3114=PLANE('',#3592);
#3115=PLANE('',#3606);
#3116=PLANE('',#3610);
#3117=PLANE('',#3614);
#3118=PLANE('',#3618);
#3119=PLANE('',#3622);
#3120=PLANE('',#3626);
#3121=PLANE('',#3630);
#3122=PLANE('',#3634);
#3123=PLANE('',#3638);
#3124=PLANE('',#3642);
#3125=PLANE('',#3646);
#3126=PLANE('',#3650);
#3127=PLANE('',#3651);
#3128=PLANE('',#3652);
#3129=PLANE('',#3657);
#3130=PLANE('',#3658);
#3131=ADVANCED_FACE('',(#281),#3003,.T.);
#3132=ADVANCED_FACE('',(#282),#3004,.T.);
#3133=ADVANCED_FACE('',(#283),#3005,.T.);
#3134=ADVANCED_FACE('',(#284),#3006,.T.);
#3135=ADVANCED_FACE('',(#285),#3007,.F.);
#3136=ADVANCED_FACE('',(#286),#3008,.T.);
#3137=ADVANCED_FACE('',(#287),#3009,.T.);
#3138=ADVANCED_FACE('',(#288),#145,.T.);
#3139=ADVANCED_FACE('',(#289),#3010,.T.);
#3140=ADVANCED_FACE('',(#290),#146,.T.);
#3141=ADVANCED_FACE('',(#291),#3011,.T.);
#3142=ADVANCED_FACE('',(#292),#3012,.T.);
#3143=ADVANCED_FACE('',(#293),#3013,.F.);
#3144=ADVANCED_FACE('',(#294),#147,.F.);
#3145=ADVANCED_FACE('',(#295),#3014,.F.);
#3146=ADVANCED_FACE('',(#296),#148,.F.);
#3147=ADVANCED_FACE('',(#297),#3015,.T.);
#3148=ADVANCED_FACE('',(#298),#3016,.F.);
#3149=ADVANCED_FACE('',(#299),#3017,.F.);
#3150=ADVANCED_FACE('',(#300),#3018,.F.);
#3151=ADVANCED_FACE('',(#301),#3019,.F.);
#3152=ADVANCED_FACE('',(#302),#3020,.F.);
#3153=ADVANCED_FACE('',(#303),#3021,.F.);
#3154=ADVANCED_FACE('',(#304),#3022,.F.);
#3155=ADVANCED_FACE('',(#305),#3023,.F.);
#3156=ADVANCED_FACE('',(#306),#3024,.F.);
#3157=ADVANCED_FACE('',(#307),#3025,.F.);
#3158=ADVANCED_FACE('',(#308),#3026,.F.);
#3159=ADVANCED_FACE('',(#309),#3027,.F.);
#3160=ADVANCED_FACE('',(#310),#3028,.F.);
#3161=ADVANCED_FACE('',(#311),#3029,.F.);
#3162=ADVANCED_FACE('',(#312),#3030,.F.);
#3163=ADVANCED_FACE('',(#313),#3031,.F.);
#3164=ADVANCED_FACE('',(#314),#3032,.F.);
#3165=ADVANCED_FACE('',(#315),#3033,.F.);
#3166=ADVANCED_FACE('',(#316),#3034,.F.);
#3167=ADVANCED_FACE('',(#317),#3035,.F.);
#3168=ADVANCED_FACE('',(#318),#3036,.F.);
#3169=ADVANCED_FACE('',(#319),#3037,.F.);
#3170=ADVANCED_FACE('',(#320),#3038,.F.);
#3171=ADVANCED_FACE('',(#321),#3039,.F.);
#3172=ADVANCED_FACE('',(#322),#3040,.F.);
#3173=ADVANCED_FACE('',(#323),#3041,.F.);
#3174=ADVANCED_FACE('',(#324),#3042,.F.);
#3175=ADVANCED_FACE('',(#325),#3043,.F.);
#3176=ADVANCED_FACE('',(#326),#3044,.F.);
#3177=ADVANCED_FACE('',(#327),#3045,.F.);
#3178=ADVANCED_FACE('',(#328),#3046,.F.);
#3179=ADVANCED_FACE('',(#329),#3047,.F.);
#3180=ADVANCED_FACE('',(#330),#3048,.F.);
#3181=ADVANCED_FACE('',(#331),#3049,.F.);
#3182=ADVANCED_FACE('',(#332),#3050,.F.);
#3183=ADVANCED_FACE('',(#333),#3051,.F.);
#3184=ADVANCED_FACE('',(#334),#3052,.F.);
#3185=ADVANCED_FACE('',(#335),#3053,.T.);
#3186=ADVANCED_FACE('',(#336),#3054,.T.);
#3187=ADVANCED_FACE('',(#337),#3055,.T.);
#3188=ADVANCED_FACE('',(#338),#3056,.T.);
#3189=ADVANCED_FACE('',(#339),#149,.T.);
#3190=ADVANCED_FACE('',(#340),#150,.T.);
#3191=ADVANCED_FACE('',(#341),#151,.T.);
#3192=ADVANCED_FACE('',(#342),#152,.T.);
#3193=ADVANCED_FACE('',(#343),#153,.T.);
#3194=ADVANCED_FACE('',(#344),#154,.T.);
#3195=ADVANCED_FACE('',(#345),#155,.T.);
#3196=ADVANCED_FACE('',(#346),#156,.T.);
#3197=ADVANCED_FACE('',(#347),#3057,.T.);
#3198=ADVANCED_FACE('',(#348),#3058,.T.);
#3199=ADVANCED_FACE('',(#349),#3059,.T.);
#3200=ADVANCED_FACE('',(#350),#3060,.T.);
#3201=ADVANCED_FACE('',(#351),#3061,.T.);
#3202=ADVANCED_FACE('',(#352),#3062,.T.);
#3203=ADVANCED_FACE('',(#353),#3063,.T.);
#3204=ADVANCED_FACE('',(#354),#3064,.T.);
#3205=ADVANCED_FACE('',(#355),#3065,.T.);
#3206=ADVANCED_FACE('',(#356),#3066,.T.);
#3207=ADVANCED_FACE('',(#357),#3067,.T.);
#3208=ADVANCED_FACE('',(#358),#3068,.T.);
#3209=ADVANCED_FACE('',(#359),#3069,.T.);
#3210=ADVANCED_FACE('',(#360),#3070,.T.);
#3211=ADVANCED_FACE('',(#361),#3071,.T.);
#3212=ADVANCED_FACE('',(#362),#3072,.T.);
#3213=ADVANCED_FACE('',(#363),#3073,.F.);
#3214=ADVANCED_FACE('',(#364),#3074,.T.);
#3215=ADVANCED_FACE('',(#365),#3075,.T.);
#3216=ADVANCED_FACE('',(#366),#157,.F.);
#3217=ADVANCED_FACE('',(#367),#3076,.T.);
#3218=ADVANCED_FACE('',(#368),#158,.T.);
#3219=ADVANCED_FACE('',(#369),#3077,.T.);
#3220=ADVANCED_FACE('',(#370),#159,.T.);
#3221=ADVANCED_FACE('',(#371),#3078,.T.);
#3222=ADVANCED_FACE('',(#372),#160,.F.);
#3223=ADVANCED_FACE('',(#373),#3079,.T.);
#3224=ADVANCED_FACE('',(#374),#3080,.T.);
#3225=ADVANCED_FACE('',(#375),#3081,.F.);
#3226=ADVANCED_FACE('',(#376),#161,.T.);
#3227=ADVANCED_FACE('',(#377),#3082,.F.);
#3228=ADVANCED_FACE('',(#378),#162,.F.);
#3229=ADVANCED_FACE('',(#379),#3083,.F.);
#3230=ADVANCED_FACE('',(#380),#163,.F.);
#3231=ADVANCED_FACE('',(#381),#3084,.F.);
#3232=ADVANCED_FACE('',(#382),#164,.T.);
#3233=ADVANCED_FACE('',(#383),#3085,.F.);
#3234=ADVANCED_FACE('',(#384),#3086,.T.);
#3235=ADVANCED_FACE('',(#385),#3087,.F.);
#3236=ADVANCED_FACE('',(#386,#99,#100),#3088,.F.);
#3237=ADVANCED_FACE('',(#387),#3089,.F.);
#3238=ADVANCED_FACE('',(#388),#3090,.F.);
#3239=ADVANCED_FACE('',(#389),#165,.T.);
#3240=ADVANCED_FACE('',(#390),#3091,.F.);
#3241=ADVANCED_FACE('',(#391,#101,#102),#3092,.F.);
#3242=ADVANCED_FACE('',(#392),#166,.T.);
#3243=ADVANCED_FACE('',(#393),#3093,.T.);
#3244=ADVANCED_FACE('',(#394),#3094,.F.);
#3245=ADVANCED_FACE('',(#395),#167,.F.);
#3246=ADVANCED_FACE('',(#396),#3095,.F.);
#3247=ADVANCED_FACE('',(#397),#168,.F.);
#3248=ADVANCED_FACE('',(#398),#3096,.F.);
#3249=ADVANCED_FACE('',(#399),#169,.F.);
#3250=ADVANCED_FACE('',(#400),#3097,.F.);
#3251=ADVANCED_FACE('',(#401),#170,.F.);
#3252=ADVANCED_FACE('',(#402),#3098,.F.);
#3253=ADVANCED_FACE('',(#403),#3099,.T.);
#3254=ADVANCED_FACE('',(#404),#3100,.T.);
#3255=ADVANCED_FACE('',(#405),#3101,.T.);
#3256=ADVANCED_FACE('',(#406),#3102,.T.);
#3257=ADVANCED_FACE('',(#407,#103,#104),#3103,.F.);
#3258=ADVANCED_FACE('',(#408),#3104,.T.);
#3259=ADVANCED_FACE('',(#409,#105,#106),#3105,.T.);
#3260=ADVANCED_FACE('',(#410),#171,.T.);
#3261=ADVANCED_FACE('',(#411),#3106,.T.);
#3262=ADVANCED_FACE('',(#412),#3107,.T.);
#3263=ADVANCED_FACE('',(#413),#3108,.F.);
#3264=ADVANCED_FACE('',(#414),#172,.F.);
#3265=ADVANCED_FACE('',(#415),#3109,.T.);
#3266=ADVANCED_FACE('',(#416),#3110,.F.);
#3267=ADVANCED_FACE('',(#417),#173,.F.);
#3268=ADVANCED_FACE('',(#418),#3111,.F.);
#3269=ADVANCED_FACE('',(#419),#174,.F.);
#3270=ADVANCED_FACE('',(#420),#3112,.F.);
#3271=ADVANCED_FACE('',(#421),#175,.F.);
#3272=ADVANCED_FACE('',(#422),#3113,.F.);
#3273=ADVANCED_FACE('',(#423),#176,.F.);
#3274=ADVANCED_FACE('',(#424),#3114,.F.);
#3275=ADVANCED_FACE('',(#425),#177,.F.);
#3276=ADVANCED_FACE('',(#426),#178,.F.);
#3277=ADVANCED_FACE('',(#427),#179,.F.);
#3278=ADVANCED_FACE('',(#428),#180,.T.);
#3279=ADVANCED_FACE('',(#429,#107),#3115,.F.);
#3280=ADVANCED_FACE('',(#430),#181,.F.);
#3281=ADVANCED_FACE('',(#431),#3116,.F.);
#3282=ADVANCED_FACE('',(#432),#182,.F.);
#3283=ADVANCED_FACE('',(#433,#108),#3117,.F.);
#3284=ADVANCED_FACE('',(#434),#183,.T.);
#3285=ADVANCED_FACE('',(#435),#3118,.F.);
#3286=ADVANCED_FACE('',(#436),#184,.T.);
#3287=ADVANCED_FACE('',(#437,#109),#3119,.F.);
#3288=ADVANCED_FACE('',(#438),#185,.T.);
#3289=ADVANCED_FACE('',(#439),#3120,.F.);
#3290=ADVANCED_FACE('',(#440),#186,.F.);
#3291=ADVANCED_FACE('',(#441,#110),#3121,.F.);
#3292=ADVANCED_FACE('',(#442),#187,.T.);
#3293=ADVANCED_FACE('',(#443),#3122,.F.);
#3294=ADVANCED_FACE('',(#444),#188,.T.);
#3295=ADVANCED_FACE('',(#445,#111),#3123,.F.);
#3296=ADVANCED_FACE('',(#446),#189,.F.);
#3297=ADVANCED_FACE('',(#447),#3124,.F.);
#3298=ADVANCED_FACE('',(#448),#190,.T.);
#3299=ADVANCED_FACE('',(#449,#112),#3125,.F.);
#3300=ADVANCED_FACE('',(#450),#191,.T.);
#3301=ADVANCED_FACE('',(#451),#3126,.F.);
#3302=ADVANCED_FACE('',(#452),#3127,.F.);
#3303=ADVANCED_FACE('',(#453),#3128,.T.);
#3304=ADVANCED_FACE('',(#454),#192,.T.);
#3305=ADVANCED_FACE('',(#455),#3129,.T.);
#3306=ADVANCED_FACE('',(#456),#3130,.F.);
#3307=CLOSED_SHELL('',(#3131,#3132,#3133,#3134,#3135,#3136,#3137,#3138,
#3139,#3140,#3141,#3142,#3143,#3144,#3145,#3146,#3147,#3148,#3149,#3150,
#3151,#3152,#3153,#3154,#3155,#3156,#3157,#3158,#3159,#3160,#3161,#3162,
#3163,#3164,#3165,#3166,#3167,#3168,#3169,#3170,#3171,#3172,#3173,#3174,
#3175,#3176,#3177,#3178,#3179,#3180,#3181,#3182,#3183,#3184,#3185,#3186,
#3187,#3188,#3189,#3190,#3191,#3192,#3193,#3194,#3195,#3196));
#3308=CLOSED_SHELL('',(#3197,#3198,#3199,#3200,#3201,#3202,#3203,#3204,
#3205,#3206,#3207,#3208,#3209,#3210,#3211,#3212,#3213,#3214,#3215,#3216,
#3217,#3218,#3219,#3220,#3221,#3222,#3223,#3224,#3225,#3226,#3227,#3228,
#3229,#3230,#3231,#3232,#3233,#3234));
#3309=CLOSED_SHELL('',(#3235,#3236,#3237,#3238,#3239,#3240,#3241,#3242,
#3243,#3244,#3245,#3246,#3247,#3248,#3249,#3250,#3251,#3252));
#3310=CLOSED_SHELL('',(#3253,#3254,#3255,#3256,#3257,#3258,#3259,#3260,
#3261,#3262,#3263,#3264,#3265,#3266,#3267,#3268,#3269,#3270,#3271,#3272,
#3273,#3274));
#3311=CLOSED_SHELL('',(#3275,#3276,#3277,#3278,#3279,#3280,#3281,#3282,
#3283,#3284,#3285,#3286,#3287,#3288,#3289,#3290,#3291,#3292,#3293,#3294,
#3295,#3296,#3297,#3298,#3299,#3300,#3301,#3302,#3303));
#3312=CLOSED_SHELL('',(#3304,#3305,#3306));
#3313=DERIVED_UNIT_ELEMENT(#3325,1.);
#3314=DERIVED_UNIT_ELEMENT(#5601,-3.);
#3315=DERIVED_UNIT_ELEMENT(#3325,1.);
#3316=DERIVED_UNIT_ELEMENT(#5601,-3.);
#3317=DERIVED_UNIT_ELEMENT(#3325,1.);
#3318=DERIVED_UNIT_ELEMENT(#5601,-3.);
#3319=DERIVED_UNIT_ELEMENT(#3325,1.);
#3320=DERIVED_UNIT_ELEMENT(#5601,-3.);
#3321=DERIVED_UNIT_ELEMENT(#3325,1.);
#3322=DERIVED_UNIT_ELEMENT(#5601,-3.);
#3323=DERIVED_UNIT_ELEMENT(#3325,1.);
#3324=DERIVED_UNIT_ELEMENT(#5601,-3.);
#3325=(
MASS_UNIT()
NAMED_UNIT(*)
SI_UNIT(.KILO.,.GRAM.)
);
#3326=DERIVED_UNIT((#3313,#3314));
#3327=DERIVED_UNIT((#3315,#3316));
#3328=DERIVED_UNIT((#3317,#3318));
#3329=DERIVED_UNIT((#3319,#3320));
#3330=DERIVED_UNIT((#3321,#3322));
#3331=DERIVED_UNIT((#3323,#3324));
#3332=MEASURE_REPRESENTATION_ITEM('density measure',
POSITIVE_RATIO_MEASURE(7850.),#3326);
#3333=MEASURE_REPRESENTATION_ITEM('density measure',
POSITIVE_RATIO_MEASURE(7850.),#3327);
#3334=MEASURE_REPRESENTATION_ITEM('density measure',
POSITIVE_RATIO_MEASURE(7850.),#3328);
#3335=MEASURE_REPRESENTATION_ITEM('density measure',
POSITIVE_RATIO_MEASURE(7850.),#3329);
#3336=MEASURE_REPRESENTATION_ITEM('density measure',
POSITIVE_RATIO_MEASURE(7850.),#3330);
#3337=MEASURE_REPRESENTATION_ITEM('density measure',
POSITIVE_RATIO_MEASURE(7850.),#3331);
#3338=PROPERTY_DEFINITION_REPRESENTATION(#3368,#3350);
#3339=PROPERTY_DEFINITION_REPRESENTATION(#3369,#3351);
#3340=PROPERTY_DEFINITION_REPRESENTATION(#3370,#3352);
#3341=PROPERTY_DEFINITION_REPRESENTATION(#3371,#3353);
#3342=PROPERTY_DEFINITION_REPRESENTATION(#3372,#3354);
#3343=PROPERTY_DEFINITION_REPRESENTATION(#3373,#3355);
#3344=PROPERTY_DEFINITION_REPRESENTATION(#3374,#3356);
#3345=PROPERTY_DEFINITION_REPRESENTATION(#3375,#3357);
#3346=PROPERTY_DEFINITION_REPRESENTATION(#3376,#3358);
#3347=PROPERTY_DEFINITION_REPRESENTATION(#3377,#3359);
#3348=PROPERTY_DEFINITION_REPRESENTATION(#3378,#3360);
#3349=PROPERTY_DEFINITION_REPRESENTATION(#3379,#3361);
#3350=REPRESENTATION('material name',(#3362),#5593);
#3351=REPRESENTATION('density',(#3332),#5593);
#3352=REPRESENTATION('material name',(#3363),#5594);
#3353=REPRESENTATION('density',(#3333),#5594);
#3354=REPRESENTATION('material name',(#3364),#5595);
#3355=REPRESENTATION('density',(#3334),#5595);
#3356=REPRESENTATION('material name',(#3365),#5596);
#3357=REPRESENTATION('density',(#3335),#5596);
#3358=REPRESENTATION('material name',(#3366),#5597);
#3359=REPRESENTATION('density',(#3336),#5597);
#3360=REPRESENTATION('material name',(#3367),#5598);
#3361=REPRESENTATION('density',(#3337),#5598);
#3362=DESCRIPTIVE_REPRESENTATION_ITEM('Steel','Steel');
#3363=DESCRIPTIVE_REPRESENTATION_ITEM('Steel','Steel');
#3364=DESCRIPTIVE_REPRESENTATION_ITEM('Steel','Steel');
#3365=DESCRIPTIVE_REPRESENTATION_ITEM('Steel','Steel');
#3366=DESCRIPTIVE_REPRESENTATION_ITEM('Steel','Steel');
#3367=DESCRIPTIVE_REPRESENTATION_ITEM('Steel','Steel');
#3368=PROPERTY_DEFINITION('material property','material name',#5649);
#3369=PROPERTY_DEFINITION('material property','density of part',#5649);
#3370=PROPERTY_DEFINITION('material property','material name',#5650);
#3371=PROPERTY_DEFINITION('material property','density of part',#5650);
#3372=PROPERTY_DEFINITION('material property','material name',#5651);
#3373=PROPERTY_DEFINITION('material property','density of part',#5651);
#3374=PROPERTY_DEFINITION('material property','material name',#5652);
#3375=PROPERTY_DEFINITION('material property','density of part',#5652);
#3376=PROPERTY_DEFINITION('material property','material name',#5653);
#3377=PROPERTY_DEFINITION('material property','density of part',#5653);
#3378=PROPERTY_DEFINITION('material property','material name',#5654);
#3379=PROPERTY_DEFINITION('material property','density of part',#5654);
#3380=AXIS2_PLACEMENT_3D('',#4639,#3681,#3682);
#3381=AXIS2_PLACEMENT_3D('',#4640,#3683,#3684);
#3382=AXIS2_PLACEMENT_3D('',#4641,#3685,#3686);
#3383=AXIS2_PLACEMENT_3D('',#4650,#3691,#3692);
#3384=AXIS2_PLACEMENT_3D('',#4659,#3697,#3698);
#3385=AXIS2_PLACEMENT_3D('',#4668,#3703,#3704);
#3386=AXIS2_PLACEMENT_3D('',#4677,#3709,#3710);
#3387=AXIS2_PLACEMENT_3D('',#4682,#3712,#3713);
#3388=AXIS2_PLACEMENT_3D('',#4722,#3734,#3735);
#3389=AXIS2_PLACEMENT_3D('',#4724,#3736,#3737);
#3390=AXIS2_PLACEMENT_3D('',#4731,#3741,#3742);
#3391=AXIS2_PLACEMENT_3D('',#4732,#3743,#3744);
#3392=AXIS2_PLACEMENT_3D('',#4738,#3748,#3749);
#3393=AXIS2_PLACEMENT_3D('',#4740,#3750,#3751);
#3394=AXIS2_PLACEMENT_3D('',#4744,#3753,#3754);
#3395=AXIS2_PLACEMENT_3D('',#4751,#3758,#3759);
#3396=AXIS2_PLACEMENT_3D('',#4752,#3760,#3761);
#3397=AXIS2_PLACEMENT_3D('',#4790,#3781,#3782);
#3398=AXIS2_PLACEMENT_3D('',#4792,#3783,#3784);
#3399=AXIS2_PLACEMENT_3D('',#4794,#3785,#3786);
#3400=AXIS2_PLACEMENT_3D('',#4796,#3788,#3789);
#3401=AXIS2_PLACEMENT_3D('',#4802,#3793,#3794);
#3402=AXIS2_PLACEMENT_3D('',#4804,#3795,#3796);
#3403=AXIS2_PLACEMENT_3D('',#4806,#3797,#3798);
#3404=AXIS2_PLACEMENT_3D('',#4808,#3800,#3801);
#3405=AXIS2_PLACEMENT_3D('',#4810,#3802,#3803);
#3406=AXIS2_PLACEMENT_3D('',#4851,#3824,#3825);
#3407=AXIS2_PLACEMENT_3D('',#4855,#3827,#3828);
#3408=AXIS2_PLACEMENT_3D('',#4859,#3831,#3832);
#3409=AXIS2_PLACEMENT_3D('',#4860,#3833,#3834);
#3410=AXIS2_PLACEMENT_3D('',#4866,#3838,#3839);
#3411=AXIS2_PLACEMENT_3D('',#4867,#3840,#3841);
#3412=AXIS2_PLACEMENT_3D('',#4869,#3842,#3843);
#3413=AXIS2_PLACEMENT_3D('',#4877,#3847,#3848);
#3414=AXIS2_PLACEMENT_3D('',#4880,#3850,#3851);
#3415=AXIS2_PLACEMENT_3D('',#4918,#3871,#3872);
#3416=AXIS2_PLACEMENT_3D('',#4922,#3874,#3875);
#3417=AXIS2_PLACEMENT_3D('',#4923,#3876,#3877);
#3418=AXIS2_PLACEMENT_3D('',#4924,#3878,#3879);
#3419=AXIS2_PLACEMENT_3D('',#4930,#3883,#3884);
#3420=AXIS2_PLACEMENT_3D('',#4931,#3885,#3886);
#3421=AXIS2_PLACEMENT_3D('',#4932,#3887,#3888);
#3422=AXIS2_PLACEMENT_3D('',#4933,#3889,#3890);
#3423=AXIS2_PLACEMENT_3D('',#4936,#3893,#3894);
#3424=AXIS2_PLACEMENT_3D('',#4939,#3897,#3898);
#3425=AXIS2_PLACEMENT_3D('',#4942,#3901,#3902);
#3426=AXIS2_PLACEMENT_3D('',#4945,#3905,#3906);
#3427=AXIS2_PLACEMENT_3D('',#4948,#3909,#3910);
#3428=AXIS2_PLACEMENT_3D('',#4951,#3913,#3914);
#3429=AXIS2_PLACEMENT_3D('',#4953,#3916,#3917);
#3430=AXIS2_PLACEMENT_3D('',#4955,#3919,#3920);
#3431=AXIS2_PLACEMENT_3D('',#4958,#3923,#3924);
#3432=AXIS2_PLACEMENT_3D('',#4960,#3926,#3927);
#3433=AXIS2_PLACEMENT_3D('',#4962,#3929,#3930);
#3434=AXIS2_PLACEMENT_3D('',#4965,#3933,#3934);
#3435=AXIS2_PLACEMENT_3D('',#4968,#3937,#3938);
#3436=AXIS2_PLACEMENT_3D('',#4970,#3940,#3941);
#3437=AXIS2_PLACEMENT_3D('',#4972,#3943,#3944);
#3438=AXIS2_PLACEMENT_3D('',#4975,#3947,#3948);
#3439=AXIS2_PLACEMENT_3D('',#4976,#3949,#3950);
#3440=AXIS2_PLACEMENT_3D('',#4979,#3953,#3954);
#3441=AXIS2_PLACEMENT_3D('',#4981,#3956,#3957);
#3442=AXIS2_PLACEMENT_3D('',#4984,#3960,#3961);
#3443=AXIS2_PLACEMENT_3D('',#4986,#3963,#3964);
#3444=AXIS2_PLACEMENT_3D('',#4988,#3966,#3967);
#3445=AXIS2_PLACEMENT_3D('',#4991,#3970,#3971);
#3446=AXIS2_PLACEMENT_3D('',#4994,#3974,#3975);
#3447=AXIS2_PLACEMENT_3D('',#4996,#3977,#3978);
#3448=AXIS2_PLACEMENT_3D('',#4998,#3980,#3981);
#3449=AXIS2_PLACEMENT_3D('',#5001,#3984,#3985);
#3450=AXIS2_PLACEMENT_3D('',#5003,#3987,#3988);
#3451=AXIS2_PLACEMENT_3D('',#5005,#3990,#3991);
#3452=AXIS2_PLACEMENT_3D('',#5007,#3993,#3994);
#3453=AXIS2_PLACEMENT_3D('',#5008,#3995,#3996);
#3454=AXIS2_PLACEMENT_3D('',#5009,#3997,#3998);
#3455=AXIS2_PLACEMENT_3D('',#5010,#3999,#4000);
#3456=AXIS2_PLACEMENT_3D('',#5011,#4001,#4002);
#3457=AXIS2_PLACEMENT_3D('',#5012,#4003,#4004);
#3458=AXIS2_PLACEMENT_3D('',#5013,#4005,#4006);
#3459=AXIS2_PLACEMENT_3D('',#5014,#4007,#4008);
#3460=AXIS2_PLACEMENT_3D('',#5015,#4009,#4010);
#3461=AXIS2_PLACEMENT_3D('',#5016,#4011,#4012);
#3462=AXIS2_PLACEMENT_3D('',#5017,#4013,#4014);
#3463=AXIS2_PLACEMENT_3D('',#5018,#4015,#4016);
#3464=AXIS2_PLACEMENT_3D('',#5019,#4017,#4018);
#3465=AXIS2_PLACEMENT_3D('',#5020,#4019,#4020);
#3466=AXIS2_PLACEMENT_3D('',#5021,#4021,#4022);
#3467=AXIS2_PLACEMENT_3D('',#5022,#4023,#4024);
#3468=AXIS2_PLACEMENT_3D('',#5023,#4025,#4026);
#3469=AXIS2_PLACEMENT_3D('',#5024,#4027,#4028);
#3470=AXIS2_PLACEMENT_3D('',#5025,#4029,#4030);
#3471=AXIS2_PLACEMENT_3D('',#5026,#4031,#4032);
#3472=AXIS2_PLACEMENT_3D('',#5027,#4033,#4034);
#3473=AXIS2_PLACEMENT_3D('',#5028,#4035,#4036);
#3474=AXIS2_PLACEMENT_3D('',#5033,#4038,#4039);
#3475=AXIS2_PLACEMENT_3D('',#5036,#4041,#4042);
#3476=AXIS2_PLACEMENT_3D('',#5037,#4043,#4044);
#3477=AXIS2_PLACEMENT_3D('',#5043,#4048,#4049);
#3478=AXIS2_PLACEMENT_3D('',#5048,#4051,#4052);
#3479=AXIS2_PLACEMENT_3D('',#5051,#4054,#4055);
#3480=AXIS2_PLACEMENT_3D('',#5052,#4056,#4057);
#3481=AXIS2_PLACEMENT_3D('',#5058,#4061,#4062);
#3482=AXIS2_PLACEMENT_3D('',#5062,#4064,#4065);
#3483=AXIS2_PLACEMENT_3D('',#5063,#4066,#4067);
#3484=AXIS2_PLACEMENT_3D('',#5064,#4068,#4069);
#3485=AXIS2_PLACEMENT_3D('',#5070,#4073,#4074);
#3486=AXIS2_PLACEMENT_3D('',#5075,#4076,#4077);
#3487=AXIS2_PLACEMENT_3D('',#5078,#4079,#4080);
#3488=AXIS2_PLACEMENT_3D('',#5079,#4081,#4082);
#3489=AXIS2_PLACEMENT_3D('',#5082,#4085,#4086);
#3490=AXIS2_PLACEMENT_3D('',#5086,#4088,#4089);
#3491=AXIS2_PLACEMENT_3D('',#5087,#4090,#4091);
#3492=AXIS2_PLACEMENT_3D('',#5088,#4092,#4093);
#3493=AXIS2_PLACEMENT_3D('',#5094,#4097,#4098);
#3494=AXIS2_PLACEMENT_3D('',#5099,#4100,#4101);
#3495=AXIS2_PLACEMENT_3D('',#5102,#4103,#4104);
#3496=AXIS2_PLACEMENT_3D('',#5103,#4105,#4106);
#3497=AXIS2_PLACEMENT_3D('',#5106,#4109,#4110);
#3498=AXIS2_PLACEMENT_3D('',#5110,#4112,#4113);
#3499=AXIS2_PLACEMENT_3D('',#5111,#4114,#4115);
#3500=AXIS2_PLACEMENT_3D('',#5112,#4116,#4117);
#3501=AXIS2_PLACEMENT_3D('',#5118,#4121,#4122);
#3502=AXIS2_PLACEMENT_3D('',#5123,#4124,#4125);
#3503=AXIS2_PLACEMENT_3D('',#5126,#4127,#4128);
#3504=AXIS2_PLACEMENT_3D('',#5127,#4129,#4130);
#3505=AXIS2_PLACEMENT_3D('',#5130,#4133,#4134);
#3506=AXIS2_PLACEMENT_3D('',#5135,#4138,#4139);
#3507=AXIS2_PLACEMENT_3D('',#5139,#4142,#4143);
#3508=AXIS2_PLACEMENT_3D('',#5142,#4146,#4147);
#3509=AXIS2_PLACEMENT_3D('',#5144,#4149,#4150);
#3510=AXIS2_PLACEMENT_3D('',#5146,#4152,#4153);
#3511=AXIS2_PLACEMENT_3D('',#5148,#4155,#4156);
#3512=AXIS2_PLACEMENT_3D('',#5150,#4158,#4159);
#3513=AXIS2_PLACEMENT_3D('',#5152,#4161,#4162);
#3514=AXIS2_PLACEMENT_3D('',#5154,#4164,#4165);
#3515=AXIS2_PLACEMENT_3D('',#5156,#4167,#4168);
#3516=AXIS2_PLACEMENT_3D('',#5160,#4171,#4172);
#3517=AXIS2_PLACEMENT_3D('',#5164,#4175,#4176);
#3518=AXIS2_PLACEMENT_3D('',#5167,#4179,#4180);
#3519=AXIS2_PLACEMENT_3D('',#5169,#4182,#4183);
#3520=AXIS2_PLACEMENT_3D('',#5171,#4185,#4186);
#3521=AXIS2_PLACEMENT_3D('',#5173,#4188,#4189);
#3522=AXIS2_PLACEMENT_3D('',#5175,#4191,#4192);
#3523=AXIS2_PLACEMENT_3D('',#5177,#4194,#4195);
#3524=AXIS2_PLACEMENT_3D('',#5179,#4197,#4198);
#3525=AXIS2_PLACEMENT_3D('',#5180,#4199,#4200);
#3526=AXIS2_PLACEMENT_3D('',#5181,#4201,#4202);
#3527=AXIS2_PLACEMENT_3D('',#5182,#4203,#4204);
#3528=AXIS2_PLACEMENT_3D('',#5183,#4205,#4206);
#3529=AXIS2_PLACEMENT_3D('',#5192,#4211,#4212);
#3530=AXIS2_PLACEMENT_3D('',#5202,#4217,#4218);
#3531=AXIS2_PLACEMENT_3D('',#5205,#4220,#4221);
#3532=AXIS2_PLACEMENT_3D('',#5210,#4223,#4224);
#3533=AXIS2_PLACEMENT_3D('',#5213,#4226,#4227);
#3534=AXIS2_PLACEMENT_3D('',#5214,#4228,#4229);
#3535=AXIS2_PLACEMENT_3D('',#5220,#4233,#4234);
#3536=AXIS2_PLACEMENT_3D('',#5226,#4238,#4239);
#3537=AXIS2_PLACEMENT_3D('',#5228,#4240,#4241);
#3538=AXIS2_PLACEMENT_3D('',#5231,#4243,#4244);
#3539=AXIS2_PLACEMENT_3D('',#5232,#4245,#4246);
#3540=AXIS2_PLACEMENT_3D('',#5238,#4250,#4251);
#3541=AXIS2_PLACEMENT_3D('',#5248,#4256,#4257);
#3542=AXIS2_PLACEMENT_3D('',#5251,#4259,#4260);
#3543=AXIS2_PLACEMENT_3D('',#5256,#4262,#4263);
#3544=AXIS2_PLACEMENT_3D('',#5259,#4265,#4266);
#3545=AXIS2_PLACEMENT_3D('',#5260,#4267,#4268);
#3546=AXIS2_PLACEMENT_3D('',#5261,#4269,#4270);
#3547=AXIS2_PLACEMENT_3D('',#5262,#4271,#4272);
#3548=AXIS2_PLACEMENT_3D('',#5263,#4273,#4274);
#3549=AXIS2_PLACEMENT_3D('',#5264,#4275,#4276);
#3550=AXIS2_PLACEMENT_3D('',#5265,#4277,#4278);
#3551=AXIS2_PLACEMENT_3D('',#5268,#4281,#4282);
#3552=AXIS2_PLACEMENT_3D('',#5270,#4284,#4285);
#3553=AXIS2_PLACEMENT_3D('',#5272,#4287,#4288);
#3554=AXIS2_PLACEMENT_3D('',#5273,#4289,#4290);
#3555=AXIS2_PLACEMENT_3D('',#5276,#4293,#4294);
#3556=AXIS2_PLACEMENT_3D('',#5278,#4296,#4297);
#3557=AXIS2_PLACEMENT_3D('',#5280,#4299,#4300);
#3558=AXIS2_PLACEMENT_3D('',#5281,#4301,#4302);
#3559=AXIS2_PLACEMENT_3D('',#5282,#4303,#4304);
#3560=AXIS2_PLACEMENT_3D('',#5287,#4306,#4307);
#3561=AXIS2_PLACEMENT_3D('',#5290,#4309,#4310);
#3562=AXIS2_PLACEMENT_3D('',#5291,#4311,#4312);
#3563=AXIS2_PLACEMENT_3D('',#5297,#4316,#4317);
#3564=AXIS2_PLACEMENT_3D('',#5302,#4319,#4320);
#3565=AXIS2_PLACEMENT_3D('',#5305,#4322,#4323);
#3566=AXIS2_PLACEMENT_3D('',#5306,#4324,#4325);
#3567=AXIS2_PLACEMENT_3D('',#5312,#4329,#4330);
#3568=AXIS2_PLACEMENT_3D('',#5321,#4335,#4336);
#3569=AXIS2_PLACEMENT_3D('',#5324,#4338,#4339);
#3570=AXIS2_PLACEMENT_3D('',#5329,#4341,#4342);
#3571=AXIS2_PLACEMENT_3D('',#5332,#4344,#4345);
#3572=AXIS2_PLACEMENT_3D('',#5333,#4346,#4347);
#3573=AXIS2_PLACEMENT_3D('',#5337,#4350,#4351);
#3574=AXIS2_PLACEMENT_3D('',#5342,#4354,#4355);
#3575=AXIS2_PLACEMENT_3D('',#5346,#4357,#4358);
#3576=AXIS2_PLACEMENT_3D('',#5350,#4360,#4361);
#3577=AXIS2_PLACEMENT_3D('',#5354,#4363,#4364);
#3578=AXIS2_PLACEMENT_3D('',#5356,#4366,#4367);
#3579=AXIS2_PLACEMENT_3D('',#5358,#4369,#4370);
#3580=AXIS2_PLACEMENT_3D('',#5362,#4373,#4374);
#3581=AXIS2_PLACEMENT_3D('',#5366,#4377,#4378);
#3582=AXIS2_PLACEMENT_3D('',#5369,#4381,#4382);
#3583=AXIS2_PLACEMENT_3D('',#5370,#4383,#4384);
#3584=AXIS2_PLACEMENT_3D('',#5371,#4385,#4386);
#3585=AXIS2_PLACEMENT_3D('',#5372,#4387,#4388);
#3586=AXIS2_PLACEMENT_3D('',#5375,#4391,#4392);
#3587=AXIS2_PLACEMENT_3D('',#5377,#4394,#4395);
#3588=AXIS2_PLACEMENT_3D('',#5379,#4397,#4398);
#3589=AXIS2_PLACEMENT_3D('',#5380,#4399,#4400);
#3590=AXIS2_PLACEMENT_3D('',#5383,#4403,#4404);
#3591=AXIS2_PLACEMENT_3D('',#5385,#4406,#4407);
#3592=AXIS2_PLACEMENT_3D('',#5387,#4409,#4410);
#3593=AXIS2_PLACEMENT_3D('',#5388,#4411,#4412);
#3594=AXIS2_PLACEMENT_3D('',#5389,#4413,#4414);
#3595=AXIS2_PLACEMENT_3D('',#5391,#4415,#4416);
#3596=AXIS2_PLACEMENT_3D('',#5394,#4418,#4419);
#3597=AXIS2_PLACEMENT_3D('',#5395,#4420,#4421);
#3598=AXIS2_PLACEMENT_3D('',#5397,#4422,#4423);
#3599=AXIS2_PLACEMENT_3D('',#5400,#4425,#4426);
#3600=AXIS2_PLACEMENT_3D('',#5401,#4427,#4428);
#3601=AXIS2_PLACEMENT_3D('',#5403,#4429,#4430);
#3602=AXIS2_PLACEMENT_3D('',#5406,#4432,#4433);
#3603=AXIS2_PLACEMENT_3D('',#5407,#4434,#4435);
#3604=AXIS2_PLACEMENT_3D('',#5410,#4436,#4437);
#3605=AXIS2_PLACEMENT_3D('',#5414,#4439,#4440);
#3606=AXIS2_PLACEMENT_3D('',#5416,#4442,#4443);
#3607=AXIS2_PLACEMENT_3D('',#5422,#4447,#4448);
#3608=AXIS2_PLACEMENT_3D('',#5424,#4449,#4450);
#3609=AXIS2_PLACEMENT_3D('',#5427,#4452,#4453);
#3610=AXIS2_PLACEMENT_3D('',#5428,#4454,#4455);
#3611=AXIS2_PLACEMENT_3D('',#5434,#4459,#4460);
#3612=AXIS2_PLACEMENT_3D('',#5436,#4461,#4462);
#3613=AXIS2_PLACEMENT_3D('',#5439,#4464,#4465);
#3614=AXIS2_PLACEMENT_3D('',#5440,#4466,#4467);
#3615=AXIS2_PLACEMENT_3D('',#5446,#4471,#4472);
#3616=AXIS2_PLACEMENT_3D('',#5448,#4473,#4474);
#3617=AXIS2_PLACEMENT_3D('',#5451,#4476,#4477);
#3618=AXIS2_PLACEMENT_3D('',#5452,#4478,#4479);
#3619=AXIS2_PLACEMENT_3D('',#5458,#4483,#4484);
#3620=AXIS2_PLACEMENT_3D('',#5460,#4485,#4486);
#3621=AXIS2_PLACEMENT_3D('',#5463,#4488,#4489);
#3622=AXIS2_PLACEMENT_3D('',#5464,#4490,#4491);
#3623=AXIS2_PLACEMENT_3D('',#5470,#4495,#4496);
#3624=AXIS2_PLACEMENT_3D('',#5472,#4497,#4498);
#3625=AXIS2_PLACEMENT_3D('',#5475,#4500,#4501);
#3626=AXIS2_PLACEMENT_3D('',#5476,#4502,#4503);
#3627=AXIS2_PLACEMENT_3D('',#5482,#4507,#4508);
#3628=AXIS2_PLACEMENT_3D('',#5484,#4509,#4510);
#3629=AXIS2_PLACEMENT_3D('',#5487,#4512,#4513);
#3630=AXIS2_PLACEMENT_3D('',#5488,#4514,#4515);
#3631=AXIS2_PLACEMENT_3D('',#5494,#4519,#4520);
#3632=AXIS2_PLACEMENT_3D('',#5496,#4521,#4522);
#3633=AXIS2_PLACEMENT_3D('',#5499,#4524,#4525);
#3634=AXIS2_PLACEMENT_3D('',#5500,#4526,#4527);
#3635=AXIS2_PLACEMENT_3D('',#5506,#4531,#4532);
#3636=AXIS2_PLACEMENT_3D('',#5508,#4533,#4534);
#3637=AXIS2_PLACEMENT_3D('',#5511,#4536,#4537);
#3638=AXIS2_PLACEMENT_3D('',#5512,#4538,#4539);
#3639=AXIS2_PLACEMENT_3D('',#5518,#4543,#4544);
#3640=AXIS2_PLACEMENT_3D('',#5520,#4545,#4546);
#3641=AXIS2_PLACEMENT_3D('',#5523,#4548,#4549);
#3642=AXIS2_PLACEMENT_3D('',#5524,#4550,#4551);
#3643=AXIS2_PLACEMENT_3D('',#5530,#4555,#4556);
#3644=AXIS2_PLACEMENT_3D('',#5532,#4557,#4558);
#3645=AXIS2_PLACEMENT_3D('',#5535,#4560,#4561);
#3646=AXIS2_PLACEMENT_3D('',#5536,#4562,#4563);
#3647=AXIS2_PLACEMENT_3D('',#5542,#4567,#4568);
#3648=AXIS2_PLACEMENT_3D('',#5544,#4569,#4570);
#3649=AXIS2_PLACEMENT_3D('',#5547,#4572,#4573);
#3650=AXIS2_PLACEMENT_3D('',#5548,#4574,#4575);
#3651=AXIS2_PLACEMENT_3D('',#5551,#4578,#4579);
#3652=AXIS2_PLACEMENT_3D('',#5552,#4580,#4581);
#3653=AXIS2_PLACEMENT_3D('',#5553,#4582,#4583);
#3654=AXIS2_PLACEMENT_3D('',#5554,#4584,#4585);
#3655=AXIS2_PLACEMENT_3D('',#5556,#4586,#4587);
#3656=AXIS2_PLACEMENT_3D('',#5559,#4589,#4590);
#3657=AXIS2_PLACEMENT_3D('',#5560,#4591,#4592);
#3658=AXIS2_PLACEMENT_3D('',#5561,#4593,#4594);
#3659=AXIS2_PLACEMENT_3D('',#5562,#4595,#4596);
#3660=AXIS2_PLACEMENT_3D('',#5563,#4597,#4598);
#3661=AXIS2_PLACEMENT_3D('',#5564,#4599,#4600);
#3662=AXIS2_PLACEMENT_3D('',#5565,#4601,#4602);
#3663=AXIS2_PLACEMENT_3D('',#5566,#4603,#4604);
#3664=AXIS2_PLACEMENT_3D('',#5567,#4605,#4606);
#3665=AXIS2_PLACEMENT_3D('',#5568,#4607,#4608);
#3666=AXIS2_PLACEMENT_3D('',#5569,#4609,#4610);
#3667=AXIS2_PLACEMENT_3D('',#5570,#4611,#4612);
#3668=AXIS2_PLACEMENT_3D('',#5571,#4613,#4614);
#3669=AXIS2_PLACEMENT_3D('',#5572,#4615,#4616);
#3670=AXIS2_PLACEMENT_3D('',#5573,#4617,#4618);
#3671=AXIS2_PLACEMENT_3D('',#5574,#4619,#4620);
#3672=AXIS2_PLACEMENT_3D('',#5575,#4621,#4622);
#3673=AXIS2_PLACEMENT_3D('',#5576,#4623,#4624);
#3674=AXIS2_PLACEMENT_3D('',#5577,#4625,#4626);
#3675=AXIS2_PLACEMENT_3D('',#5578,#4627,#4628);
#3676=AXIS2_PLACEMENT_3D('',#5579,#4629,#4630);
#3677=AXIS2_PLACEMENT_3D('',#5580,#4631,#4632);
#3678=AXIS2_PLACEMENT_3D('',#5581,#4633,#4634);
#3679=AXIS2_PLACEMENT_3D('',#5582,#4635,#4636);
#3680=AXIS2_PLACEMENT_3D('',#5583,#4637,#4638);
#3681=DIRECTION('axis',(0.,0.,1.));
#3682=DIRECTION('refdir',(1.,0.,0.));
#3683=DIRECTION('axis',(0.,0.,1.));
#3684=DIRECTION('refdir',(1.,0.,0.));
#3685=DIRECTION('center_axis',(-9.01019857023267E-31,-1.,0.));
#3686=DIRECTION('ref_axis',(1.,-9.01019857023267E-31,0.));
#3687=DIRECTION('',(0.,0.,-1.));
#3688=DIRECTION('',(-1.,9.01019857023267E-31,0.));
#3689=DIRECTION('',(0.,0.,-1.));
#3690=DIRECTION('',(1.,-9.01019857023267E-31,0.));
#3691=DIRECTION('center_axis',(0.,-1.,0.));
#3692=DIRECTION('ref_axis',(0.,0.,-1.));
#3693=DIRECTION('',(0.,0.,-1.));
#3694=DIRECTION('',(-1.,0.,0.));
#3695=DIRECTION('',(0.,0.,-1.));
#3696=DIRECTION('',(1.,0.,0.));
#3697=DIRECTION('center_axis',(0.,0.,-1.));
#3698=DIRECTION('ref_axis',(-1.,0.,0.));
#3699=DIRECTION('',(0.,1.,0.));
#3700=DIRECTION('',(-1.,0.,0.));
#3701=DIRECTION('',(0.,1.,0.));
#3702=DIRECTION('',(1.,0.,0.));
#3703=DIRECTION('center_axis',(0.,0.,1.));
#3704=DIRECTION('ref_axis',(1.,0.,0.));
#3705=DIRECTION('',(-3.46944695195361E-16,-1.,0.));
#3706=DIRECTION('',(1.,-9.01019857023267E-31,0.));
#3707=DIRECTION('',(-3.46944695195361E-16,-1.,0.));
#3708=DIRECTION('',(-1.,0.,0.));
#3709=DIRECTION('center_axis',(1.,-3.46944695195361E-16,0.));
#3710=DIRECTION('ref_axis',(3.46944695195361E-16,1.,0.));
#3711=DIRECTION('',(-3.46944695195361E-16,-1.,0.));
#3712=DIRECTION('center_axis',(-1.,3.46944695195361E-16,0.));
#3713=DIRECTION('ref_axis',(3.46944695195361E-16,1.,0.));
#3714=DIRECTION('',(0.,0.,-1.));
#3715=DIRECTION('',(2.4532694666934E-16,0.707106781186549,0.707106781186546));
#3716=DIRECTION('',(3.46944695195361E-16,1.,4.3841477367998E-16));
#3717=DIRECTION('',(2.27580604085849E-16,0.655956431204979,0.754798754874985));
#3718=DIRECTION('',(0.,0.,1.));
#3719=DIRECTION('',(2.4532694666934E-16,0.707106781186547,0.707106781186547));
#3720=DIRECTION('',(3.46944695195361E-16,1.,0.));
#3721=DIRECTION('',(0.,0.,1.));
#3722=DIRECTION('',(-3.46944695195361E-16,-1.,0.));
#3723=DIRECTION('',(-2.4532694666934E-16,-0.707106781186548,0.707106781186547));
#3724=DIRECTION('',(0.,0.,1.));
#3725=DIRECTION('',(2.4532694666934E-16,0.707106781186547,0.707106781186547));
#3726=DIRECTION('',(3.46944695195361E-16,1.,0.));
#3727=DIRECTION('',(0.,0.,1.));
#3728=DIRECTION('',(-3.46944695195361E-16,-1.,0.));
#3729=DIRECTION('',(-2.4532694666934E-16,-0.707106781186548,0.707106781186547));
#3730=DIRECTION('',(0.,-8.15936190770267E-17,1.));
#3731=DIRECTION('',(-1.82277714383761E-16,-0.525379741809059,0.85086786688454));
#3732=DIRECTION('',(-3.46944695195361E-16,-1.,0.));
#3733=DIRECTION('',(-2.4532694666934E-16,-0.707106781186548,0.707106781186547));
#3734=DIRECTION('center_axis',(-1.,3.46944695195361E-16,0.));
#3735=DIRECTION('ref_axis',(3.46944695195361E-16,1.,0.));
#3736=DIRECTION('center_axis',(-1.,3.46944695195361E-16,0.));
#3737=DIRECTION('ref_axis',(3.46944695195361E-16,1.,0.));
#3738=DIRECTION('',(2.05674862010263E-16,0.592817428421694,-0.805336883893622));
#3739=DIRECTION('',(0.,0.,-1.));
#3740=DIRECTION('',(-2.05674862010263E-16,-0.592817428421694,-0.805336883893622));
#3741=DIRECTION('center_axis',(-1.,3.46944695195361E-16,0.));
#3742=DIRECTION('ref_axis',(3.46944695195361E-16,1.,8.67361737988404E-16));
#3743=DIRECTION('center_axis',(-9.01019857023267E-31,-1.,0.));
#3744=DIRECTION('ref_axis',(1.,-9.01019857023267E-31,0.));
#3745=DIRECTION('',(1.,-9.01019857023267E-31,0.));
#3746=DIRECTION('',(0.,0.,-1.));
#3747=DIRECTION('',(-1.,9.01019857023267E-31,0.));
#3748=DIRECTION('center_axis',(1.,-3.46944695195361E-16,0.));
#3749=DIRECTION('ref_axis',(3.46944695195361E-16,1.,0.));
#3750=DIRECTION('center_axis',(1.,-3.46944695195361E-16,0.));
#3751=DIRECTION('ref_axis',(3.46944695195361E-16,1.,0.));
#3752=DIRECTION('',(-3.46944695195361E-16,-1.,0.));
#3753=DIRECTION('center_axis',(1.,-3.46944695195361E-16,0.));
#3754=DIRECTION('ref_axis',(3.46944695195361E-16,1.,0.));
#3755=DIRECTION('',(0.,0.592817428421694,0.805336883893622));
#3756=DIRECTION('',(0.,0.,-1.));
#3757=DIRECTION('',(0.,-0.592817428421694,0.805336883893622));
#3758=DIRECTION('center_axis',(1.,-3.46944695195361E-16,0.));
#3759=DIRECTION('ref_axis',(3.46944695195361E-16,1.,0.));
#3760=DIRECTION('center_axis',(1.,-3.46944695195361E-16,0.));
#3761=DIRECTION('ref_axis',(3.46944695195361E-16,1.,0.));
#3762=DIRECTION('',(2.4532694666934E-16,0.707106781186548,-0.707106781186547));
#3763=DIRECTION('',(0.,1.,0.));
#3764=DIRECTION('',(0.,0.525379741809059,-0.85086786688454));
#3765=DIRECTION('',(0.,8.15936190770267E-17,-1.));
#3766=DIRECTION('',(2.4532694666934E-16,0.707106781186548,-0.707106781186547));
#3767=DIRECTION('',(0.,1.,0.));
#3768=DIRECTION('',(0.,0.,-1.));
#3769=DIRECTION('',(0.,-1.,0.));
#3770=DIRECTION('',(-2.4532694666934E-16,-0.707106781186547,-0.707106781186547));
#3771=DIRECTION('',(0.,0.,-1.));
#3772=DIRECTION('',(2.4532694666934E-16,0.707106781186548,-0.707106781186547));
#3773=DIRECTION('',(0.,1.,0.));
#3774=DIRECTION('',(0.,0.,-1.));
#3775=DIRECTION('',(0.,-1.,0.));
#3776=DIRECTION('',(-2.4532694666934E-16,-0.707106781186547,-0.707106781186547));
#3777=DIRECTION('',(0.,0.,-1.));
#3778=DIRECTION('',(0.,-0.655956431204979,-0.754798754874985));
#3779=DIRECTION('',(0.,-1.,-4.3841477367998E-16));
#3780=DIRECTION('',(-2.4532694666934E-16,-0.707106781186549,-0.707106781186546));
#3781=DIRECTION('center_axis',(0.,0.,-1.));
#3782=DIRECTION('ref_axis',(-1.,0.,0.));
#3783=DIRECTION('center_axis',(-2.37922000563897E-14,0.805336883893611,
0.59281742842171));
#3784=DIRECTION('ref_axis',(4.37979299315037E-14,-0.59281742842171,0.805336883893611));
#3785=DIRECTION('center_axis',(3.26041260031985E-15,0.805336883893623,-0.592817428421693));
#3786=DIRECTION('ref_axis',(7.54167563526444E-14,0.592817428421693,0.805336883893623));
#3787=DIRECTION('',(0.,0.,-1.));
#3788=DIRECTION('center_axis',(0.,1.,0.));
#3789=DIRECTION('ref_axis',(0.,0.,1.));
#3790=DIRECTION('',(-1.,0.,0.));
#3791=DIRECTION('',(1.,0.,0.));
#3792=DIRECTION('',(0.,0.,-1.));
#3793=DIRECTION('center_axis',(0.,0.,-1.));
#3794=DIRECTION('ref_axis',(-1.,0.,0.));
#3795=DIRECTION('center_axis',(-1.44515585527699E-14,0.805336883893626,
0.59281742842169));
#3796=DIRECTION('ref_axis',(8.24431622240136E-14,-0.59281742842169,0.805336883893626));
#3797=DIRECTION('center_axis',(-4.05348593553306E-15,0.805336883893625,
-0.592817428421691));
#3798=DIRECTION('ref_axis',(2.27187123174103E-14,0.59281742842169,0.805336883893625));
#3799=DIRECTION('',(0.,0.,-1.));
#3800=DIRECTION('center_axis',(-1.,0.,0.));
#3801=DIRECTION('ref_axis',(0.,0.,1.));
#3802=DIRECTION('center_axis',(-1.,0.,0.));
#3803=DIRECTION('ref_axis',(0.,0.,1.));
#3804=DIRECTION('',(0.,0.,-1.));
#3805=DIRECTION('',(0.,0.707106781186549,0.707106781186546));
#3806=DIRECTION('',(0.,-1.,-4.3841477367998E-16));
#3807=DIRECTION('',(0.,-0.655956431204979,-0.754798754874985));
#3808=DIRECTION('',(0.,0.,-1.));
#3809=DIRECTION('',(0.,0.707106781186547,0.707106781186547));
#3810=DIRECTION('',(0.,-1.,0.));
#3811=DIRECTION('',(0.,0.,-1.));
#3812=DIRECTION('',(0.,1.,0.));
#3813=DIRECTION('',(0.,-0.707106781186548,0.707106781186547));
#3814=DIRECTION('',(0.,0.,-1.));
#3815=DIRECTION('',(0.,0.707106781186547,0.707106781186547));
#3816=DIRECTION('',(0.,-1.,0.));
#3817=DIRECTION('',(0.,0.,-1.));
#3818=DIRECTION('',(0.,1.,0.));
#3819=DIRECTION('',(0.,-0.707106781186548,0.707106781186547));
#3820=DIRECTION('',(0.,8.15936190770267E-17,-1.));
#3821=DIRECTION('',(0.,0.525379741809059,-0.85086786688454));
#3822=DIRECTION('',(0.,1.,0.));
#3823=DIRECTION('',(0.,-0.707106781186548,0.707106781186547));
#3824=DIRECTION('center_axis',(-1.,0.,0.));
#3825=DIRECTION('ref_axis',(0.,0.,1.));
#3826=DIRECTION('',(0.,1.,0.));
#3827=DIRECTION('center_axis',(-1.,0.,0.));
#3828=DIRECTION('ref_axis',(0.,0.,1.));
#3829=DIRECTION('',(0.,-0.592817428421694,0.805336883893622));
#3830=DIRECTION('',(0.,0.592817428421694,0.805336883893622));
#3831=DIRECTION('center_axis',(-1.,0.,0.));
#3832=DIRECTION('ref_axis',(0.,0.,1.));
#3833=DIRECTION('center_axis',(0.,-1.,0.));
#3834=DIRECTION('ref_axis',(0.,0.,-1.));
#3835=DIRECTION('',(1.,0.,0.));
#3836=DIRECTION('',(0.,0.,-1.));
#3837=DIRECTION('',(-1.,0.,0.));
#3838=DIRECTION('center_axis',(-1.,0.,0.));
#3839=DIRECTION('ref_axis',(0.,0.,1.));
#3840=DIRECTION('center_axis',(1.,0.,0.));
#3841=DIRECTION('ref_axis',(0.,0.,1.));
#3842=DIRECTION('center_axis',(1.,0.,0.));
#3843=DIRECTION('ref_axis',(0.,0.,1.));
#3844=DIRECTION('',(0.,0.592817428421694,0.805336883893622));
#3845=DIRECTION('',(0.,0.,-1.));
#3846=DIRECTION('',(0.,-0.592817428421694,0.805336883893622));
#3847=DIRECTION('center_axis',(1.,0.,0.));
#3848=DIRECTION('ref_axis',(0.,1.80411241501588E-14,1.));
#3849=DIRECTION('',(0.,1.,0.));
#3850=DIRECTION('center_axis',(1.,0.,0.));
#3851=DIRECTION('ref_axis',(0.,0.,1.));
#3852=DIRECTION('',(0.,0.707106781186548,-0.707106781186547));
#3853=DIRECTION('',(0.,1.,0.));
#3854=DIRECTION('',(0.,0.525379741809059,-0.85086786688454));
#3855=DIRECTION('',(0.,8.15936190770267E-17,-1.));
#3856=DIRECTION('',(0.,0.707106781186548,-0.707106781186547));
#3857=DIRECTION('',(0.,1.,0.));
#3858=DIRECTION('',(0.,0.,-1.));
#3859=DIRECTION('',(0.,-1.,0.));
#3860=DIRECTION('',(0.,-0.707106781186547,-0.707106781186547));
#3861=DIRECTION('',(0.,0.,-1.));
#3862=DIRECTION('',(0.,0.707106781186548,-0.707106781186547));
#3863=DIRECTION('',(0.,1.,0.));
#3864=DIRECTION('',(0.,0.,-1.));
#3865=DIRECTION('',(0.,-1.,0.));
#3866=DIRECTION('',(0.,-0.707106781186547,-0.707106781186547));
#3867=DIRECTION('',(0.,0.,-1.));
#3868=DIRECTION('',(0.,-0.655956431204979,-0.754798754874985));
#3869=DIRECTION('',(0.,-1.,-4.3841477367998E-16));
#3870=DIRECTION('',(0.,-0.707106781186549,-0.707106781186546));
#3871=DIRECTION('center_axis',(0.,0.,-1.));
#3872=DIRECTION('ref_axis',(-1.,0.,0.));
#3873=DIRECTION('',(0.,0.,-1.));
#3874=DIRECTION('center_axis',(-6.87444778888498E-14,0.805336883893647,
0.592817428421661));
#3875=DIRECTION('ref_axis',(4.06950357233023E-13,-0.592817428421661,0.805336883893647));
#3876=DIRECTION('center_axis',(2.2006022666971E-14,0.805336883893619,-0.592817428421699));
#3877=DIRECTION('ref_axis',(1.87317276168279E-13,0.592817428421699,0.805336883893618));
#3878=DIRECTION('center_axis',(0.,1.,0.));
#3879=DIRECTION('ref_axis',(0.,0.,1.));
#3880=DIRECTION('',(0.,0.,-1.));
#3881=DIRECTION('',(-1.,0.,0.));
#3882=DIRECTION('',(1.,0.,0.));
#3883=DIRECTION('center_axis',(0.,0.,-1.));
#3884=DIRECTION('ref_axis',(-1.,0.,0.));
#3885=DIRECTION('center_axis',(-5.02438393635322E-14,0.805336883893605,
0.592817428421718));
#3886=DIRECTION('ref_axis',(1.40144780436978E-12,-0.592817428421718,0.805336883893605));
#3887=DIRECTION('center_axis',(-8.56871679067861E-15,0.805336883893636,
-0.592817428421675));
#3888=DIRECTION('ref_axis',(1.35125821358047E-13,0.592817428421675,0.805336883893636));
#3889=DIRECTION('center_axis',(0.,0.,1.));
#3890=DIRECTION('ref_axis',(1.,0.,0.));
#3891=DIRECTION('',(1.,0.,0.));
#3892=DIRECTION('',(-1.,0.,0.));
#3893=DIRECTION('center_axis',(0.,0.,1.));
#3894=DIRECTION('ref_axis',(1.,0.,0.));
#3895=DIRECTION('',(-1.,9.01019857023267E-31,0.));
#3896=DIRECTION('',(1.,0.,0.));
#3897=DIRECTION('center_axis',(0.,-0.805336883893622,0.592817428421694));
#3898=DIRECTION('ref_axis',(0.,-0.592817428421694,-0.805336883893622));
#3899=DIRECTION('',(-1.,0.,0.));
#3900=DIRECTION('',(-1.,0.,0.));
#3901=DIRECTION('center_axis',(0.,-0.805336883893622,-0.592817428421694));
#3902=DIRECTION('ref_axis',(0.,0.592817428421694,-0.805336883893622));
#3903=DIRECTION('',(1.,0.,0.));
#3904=DIRECTION('',(1.,0.,0.));
#3905=DIRECTION('center_axis',(0.,4.3841477367998E-16,-1.));
#3906=DIRECTION('ref_axis',(0.,1.,4.3841477367998E-16));
#3907=DIRECTION('',(1.,0.,0.));
#3908=DIRECTION('',(-1.,0.,0.));
#3909=DIRECTION('center_axis',(0.,0.,1.));
#3910=DIRECTION('ref_axis',(1.,0.,0.));
#3911=DIRECTION('',(-1.,0.,0.));
#3912=DIRECTION('',(-1.,0.,0.));
#3913=DIRECTION('center_axis',(0.,0.85086786688454,0.525379741809059));
#3914=DIRECTION('ref_axis',(0.,-0.525379741809059,0.85086786688454));
#3915=DIRECTION('',(-1.,0.,0.));
#3916=DIRECTION('center_axis',(0.,1.,8.15936190770267E-17));
#3917=DIRECTION('ref_axis',(0.,-8.15936190770267E-17,1.));
#3918=DIRECTION('',(1.,0.,0.));
#3919=DIRECTION('center_axis',(0.,0.,1.));
#3920=DIRECTION('ref_axis',(1.,0.,0.));
#3921=DIRECTION('',(-1.,0.,0.));
#3922=DIRECTION('',(-1.,0.,0.));
#3923=DIRECTION('center_axis',(0.,1.,0.));
#3924=DIRECTION('ref_axis',(0.,0.,1.));
#3925=DIRECTION('',(-1.,0.,0.));
#3926=DIRECTION('center_axis',(0.,0.,-1.));
#3927=DIRECTION('ref_axis',(-1.,0.,0.));
#3928=DIRECTION('',(1.,0.,0.));
#3929=DIRECTION('center_axis',(0.,1.,0.));
#3930=DIRECTION('ref_axis',(0.,0.,1.));
#3931=DIRECTION('',(1.,0.,0.));
#3932=DIRECTION('',(-1.,0.,0.));
#3933=DIRECTION('center_axis',(0.,0.,1.));
#3934=DIRECTION('ref_axis',(1.,0.,0.));
#3935=DIRECTION('',(-1.,0.,0.));
#3936=DIRECTION('',(-1.,0.,0.));
#3937=DIRECTION('center_axis',(0.,1.,0.));
#3938=DIRECTION('ref_axis',(0.,0.,1.));
#3939=DIRECTION('',(-1.,0.,0.));
#3940=DIRECTION('center_axis',(0.,0.,-1.));
#3941=DIRECTION('ref_axis',(-1.,0.,0.));
#3942=DIRECTION('',(1.,0.,0.));
#3943=DIRECTION('center_axis',(0.,1.,0.));
#3944=DIRECTION('ref_axis',(0.,0.,1.));
#3945=DIRECTION('',(-1.,0.,0.));
#3946=DIRECTION('',(-1.,0.,0.));
#3947=DIRECTION('center_axis',(0.,0.754798754874985,-0.655956431204979));
#3948=DIRECTION('ref_axis',(0.,0.655956431204979,0.754798754874985));
#3949=DIRECTION('center_axis',(0.,0.754798754874985,-0.655956431204979));
#3950=DIRECTION('ref_axis',(0.,0.655956431204979,0.754798754874985));
#3951=DIRECTION('',(-1.,0.,0.));
#3952=DIRECTION('',(-1.,0.,0.));
#3953=DIRECTION('center_axis',(0.,1.,0.));
#3954=DIRECTION('ref_axis',(0.,0.,1.));
#3955=DIRECTION('',(-1.,0.,0.));
#3956=DIRECTION('center_axis',(0.,0.,-1.));
#3957=DIRECTION('ref_axis',(-1.,0.,0.));
#3958=DIRECTION('',(1.,0.,0.));
#3959=DIRECTION('',(-1.,0.,0.));
#3960=DIRECTION('center_axis',(0.,1.,0.));
#3961=DIRECTION('ref_axis',(0.,0.,1.));
#3962=DIRECTION('',(-1.,0.,0.));
#3963=DIRECTION('center_axis',(0.,0.,1.));
#3964=DIRECTION('ref_axis',(1.,0.,0.));
#3965=DIRECTION('',(-1.,0.,0.));
#3966=DIRECTION('center_axis',(0.,1.,0.));
#3967=DIRECTION('ref_axis',(0.,0.,1.));
#3968=DIRECTION('',(1.,0.,0.));
#3969=DIRECTION('',(-1.,0.,0.));
#3970=DIRECTION('center_axis',(0.,0.,-1.));
#3971=DIRECTION('ref_axis',(-1.,0.,0.));
#3972=DIRECTION('',(1.,0.,0.));
#3973=DIRECTION('',(-1.,0.,0.));
#3974=DIRECTION('center_axis',(0.,1.,0.));
#3975=DIRECTION('ref_axis',(0.,0.,1.));
#3976=DIRECTION('',(-1.,0.,0.));
#3977=DIRECTION('center_axis',(0.,0.,1.));
#3978=DIRECTION('ref_axis',(1.,0.,0.));
#3979=DIRECTION('',(-1.,0.,0.));
#3980=DIRECTION('center_axis',(0.,1.,8.15936190770267E-17));
#3981=DIRECTION('ref_axis',(0.,-8.15936190770267E-17,1.));
#3982=DIRECTION('',(1.,0.,0.));
#3983=DIRECTION('',(-1.,0.,0.));
#3984=DIRECTION('center_axis',(0.,0.85086786688454,0.525379741809059));
#3985=DIRECTION('ref_axis',(0.,-0.525379741809059,0.85086786688454));
#3986=DIRECTION('',(-1.,0.,0.));
#3987=DIRECTION('center_axis',(0.,0.,1.));
#3988=DIRECTION('ref_axis',(1.,0.,0.));
#3989=DIRECTION('',(-1.,9.01019857023267E-31,0.));
#3990=DIRECTION('center_axis',(0.,4.3841477367998E-16,-1.));
#3991=DIRECTION('ref_axis',(0.,1.,4.3841477367998E-16));
#3992=DIRECTION('',(1.,-9.01019857023267E-31,0.));
#3993=DIRECTION('center_axis',(0.,0.707106781186548,-0.707106781186548));
#3994=DIRECTION('ref_axis',(-1.,0.,0.));
#3995=DIRECTION('center_axis',(0.,0.707106781186547,0.707106781186548));
#3996=DIRECTION('ref_axis',(-1.,0.,0.));
#3997=DIRECTION('center_axis',(0.,0.707106781186548,-0.707106781186548));
#3998=DIRECTION('ref_axis',(-1.,0.,0.));
#3999=DIRECTION('center_axis',(0.,0.707106781186547,0.707106781186548));
#4000=DIRECTION('ref_axis',(-1.,0.,0.));
#4001=DIRECTION('center_axis',(0.,0.707106781186548,-0.707106781186548));
#4002=DIRECTION('ref_axis',(-1.,0.,0.));
#4003=DIRECTION('center_axis',(0.,0.707106781186547,0.707106781186548));
#4004=DIRECTION('ref_axis',(-1.,0.,0.));
#4005=DIRECTION('center_axis',(0.,0.707106781186548,-0.707106781186548));
#4006=DIRECTION('ref_axis',(-1.,0.,0.));
#4007=DIRECTION('center_axis',(0.,0.707106781186547,0.707106781186548));
#4008=DIRECTION('ref_axis',(-1.,0.,0.));
#4009=DIRECTION('center_axis',(0.,-0.707106781186547,-0.707106781186548));
#4010=DIRECTION('ref_axis',(1.,0.,0.));
#4011=DIRECTION('center_axis',(0.,-0.707106781186546,0.707106781186549));
#4012=DIRECTION('ref_axis',(1.,0.,0.));
#4013=DIRECTION('center_axis',(-6.37117250884884E-31,-0.707106781186546,
0.707106781186549));
#4014=DIRECTION('ref_axis',(1.,-9.01019857023267E-31,3.65180529852271E-47));
#4015=DIRECTION('center_axis',(-6.37117250884885E-31,-0.707106781186547,
-0.707106781186548));
#4016=DIRECTION('ref_axis',(1.,-9.01019857023266E-31,5.15319092140731E-47));
#4017=DIRECTION('center_axis',(-1.,0.,0.));
#4018=DIRECTION('ref_axis',(0.,0.,1.));
#4019=DIRECTION('center_axis',(1.,0.,0.));
#4020=DIRECTION('ref_axis',(0.,0.,-1.));
#4021=DIRECTION('center_axis',(1.,-9.01019857023267E-31,0.));
#4022=DIRECTION('ref_axis',(9.01019857023267E-31,1.,0.));
#4023=DIRECTION('center_axis',(1.,0.,0.));
#4024=DIRECTION('ref_axis',(0.,0.,-1.));
#4025=DIRECTION('center_axis',(-1.,9.01019857023267E-31,0.));
#4026=DIRECTION('ref_axis',(-9.01019857023267E-31,-1.,0.));
#4027=DIRECTION('center_axis',(-1.,0.,0.));
#4028=DIRECTION('ref_axis',(0.,0.,1.));
#4029=DIRECTION('center_axis',(-1.,0.,0.));
#4030=DIRECTION('ref_axis',(0.,0.,1.));
#4031=DIRECTION('center_axis',(-1.,0.,0.));
#4032=DIRECTION('ref_axis',(0.,0.,1.));
#4033=DIRECTION('axis',(0.,0.,1.));
#4034=DIRECTION('refdir',(1.,0.,0.));
#4035=DIRECTION('center_axis',(0.,0.,1.));
#4036=DIRECTION('ref_axis',(1.,0.,0.));
#4037=DIRECTION('',(1.,0.,0.));
#4038=DIRECTION('center_axis',(0.,0.,1.));
#4039=DIRECTION('ref_axis',(-1.,0.,0.));
#4040=DIRECTION('',(0.,1.,0.));
#4041=DIRECTION('center_axis',(0.,0.,1.));
#4042=DIRECTION('ref_axis',(1.,0.,0.));
#4043=DIRECTION('center_axis',(0.,0.,1.));
#4044=DIRECTION('ref_axis',(1.,0.,0.));
#4045=DIRECTION('',(0.,1.,0.));
#4046=DIRECTION('',(0.,1.,0.));
#4047=DIRECTION('',(-1.,0.,0.));
#4048=DIRECTION('center_axis',(0.,0.,-1.));
#4049=DIRECTION('ref_axis',(-1.,0.,0.));
#4050=DIRECTION('',(0.,-1.,0.));
#4051=DIRECTION('center_axis',(0.,0.,1.));
#4052=DIRECTION('ref_axis',(-1.,0.,0.));
#4053=DIRECTION('',(-1.,0.,0.));
#4054=DIRECTION('center_axis',(0.,0.,1.));
#4055=DIRECTION('ref_axis',(1.,0.,0.));
#4056=DIRECTION('center_axis',(0.,0.,-1.));
#4057=DIRECTION('ref_axis',(-1.,0.,0.));
#4058=DIRECTION('',(1.,0.,0.));
#4059=DIRECTION('',(1.,0.,0.));
#4060=DIRECTION('',(0.,1.,0.));
#4061=DIRECTION('center_axis',(0.,0.,1.));
#4062=DIRECTION('ref_axis',(1.,0.,0.));
#4063=DIRECTION('',(0.,-1.,0.));
#4064=DIRECTION('center_axis',(0.,0.,-1.));
#4065=DIRECTION('ref_axis',(1.,0.,0.));
#4066=DIRECTION('center_axis',(0.,0.,-1.));
#4067=DIRECTION('ref_axis',(1.,0.,0.));
#4068=DIRECTION('center_axis',(0.,0.,1.));
#4069=DIRECTION('ref_axis',(1.,0.,0.));
#4070=DIRECTION('',(1.,0.,0.));
#4071=DIRECTION('',(1.,0.,0.));
#4072=DIRECTION('',(0.,1.,0.));
#4073=DIRECTION('center_axis',(0.,0.,-1.));
#4074=DIRECTION('ref_axis',(-1.,0.,0.));
#4075=DIRECTION('',(1.,0.,0.));
#4076=DIRECTION('center_axis',(0.,0.,-1.));
#4077=DIRECTION('ref_axis',(1.,0.,0.));
#4078=DIRECTION('',(0.,1.,0.));
#4079=DIRECTION('center_axis',(0.,0.,-1.));
#4080=DIRECTION('ref_axis',(1.,0.,0.));
#4081=DIRECTION('center_axis',(0.,0.,-1.));
#4082=DIRECTION('ref_axis',(-1.,0.,0.));
#4083=DIRECTION('',(0.,1.,0.));
#4084=DIRECTION('',(0.,1.,0.));
#4085=DIRECTION('center_axis',(0.,0.,1.));
#4086=DIRECTION('ref_axis',(1.,0.,0.));
#4087=DIRECTION('',(-1.,0.,0.));
#4088=DIRECTION('center_axis',(0.,0.,-1.));
#4089=DIRECTION('ref_axis',(1.,0.,0.));
#4090=DIRECTION('center_axis',(0.,0.,-1.));
#4091=DIRECTION('ref_axis',(1.,0.,0.));
#4092=DIRECTION('center_axis',(0.,0.,1.));
#4093=DIRECTION('ref_axis',(1.,0.,0.));
#4094=DIRECTION('',(0.,-1.,0.));
#4095=DIRECTION('',(0.,-1.,0.));
#4096=DIRECTION('',(1.,-6.82961998416066E-16,0.));
#4097=DIRECTION('center_axis',(0.,0.,-1.));
#4098=DIRECTION('ref_axis',(-1.,0.,0.));
#4099=DIRECTION('',(0.,-1.,0.));
#4100=DIRECTION('center_axis',(0.,0.,-1.));
#4101=DIRECTION('ref_axis',(1.,0.,0.));
#4102=DIRECTION('',(1.,0.,0.));
#4103=DIRECTION('center_axis',(0.,0.,-1.));
#4104=DIRECTION('ref_axis',(1.,0.,0.));
#4105=DIRECTION('center_axis',(0.,0.,-1.));
#4106=DIRECTION('ref_axis',(-1.,0.,0.));
#4107=DIRECTION('',(1.,0.,0.));
#4108=DIRECTION('',(1.,0.,0.));
#4109=DIRECTION('center_axis',(0.,0.,1.));
#4110=DIRECTION('ref_axis',(1.,0.,0.));
#4111=DIRECTION('',(0.,-1.,0.));
#4112=DIRECTION('center_axis',(0.,0.,1.));
#4113=DIRECTION('ref_axis',(-1.,0.,0.));
#4114=DIRECTION('center_axis',(0.,0.,1.));
#4115=DIRECTION('ref_axis',(1.,0.,0.));
#4116=DIRECTION('center_axis',(0.,0.,1.));
#4117=DIRECTION('ref_axis',(1.,0.,0.));
#4118=DIRECTION('',(1.,0.,0.));
#4119=DIRECTION('',(1.,0.,0.));
#4120=DIRECTION('',(0.,-1.,0.));
#4121=DIRECTION('center_axis',(0.,0.,-1.));
#4122=DIRECTION('ref_axis',(-1.,0.,0.));
#4123=DIRECTION('',(-1.,6.82961998416066E-16,0.));
#4124=DIRECTION('center_axis',(0.,0.,1.));
#4125=DIRECTION('ref_axis',(-1.,0.,0.));
#4126=DIRECTION('',(0.,1.,0.));
#4127=DIRECTION('center_axis',(0.,0.,1.));
#4128=DIRECTION('ref_axis',(1.,0.,0.));
#4129=DIRECTION('center_axis',(0.,0.,-1.));
#4130=DIRECTION('ref_axis',(-1.,0.,0.));
#4131=DIRECTION('',(0.,-1.,0.));
#4132=DIRECTION('',(0.,-1.,0.));
#4133=DIRECTION('center_axis',(0.,1.,0.));
#4134=DIRECTION('ref_axis',(0.,0.,1.));
#4135=DIRECTION('',(1.,0.,0.));
#4136=DIRECTION('',(0.,0.,-1.));
#4137=DIRECTION('',(0.,0.,-1.));
#4138=DIRECTION('center_axis',(1.,0.,0.));
#4139=DIRECTION('ref_axis',(0.,0.,-1.));
#4140=DIRECTION('',(0.,-1.,0.));
#4141=DIRECTION('',(0.,0.,-1.));
#4142=DIRECTION('center_axis',(0.,1.,0.));
#4143=DIRECTION('ref_axis',(0.,0.,1.));
#4144=DIRECTION('',(1.,0.,0.));
#4145=DIRECTION('',(0.,0.,-1.));
#4146=DIRECTION('center_axis',(0.,0.,-1.));
#4147=DIRECTION('ref_axis',(-1.,0.,0.));
#4148=DIRECTION('',(0.,0.,-1.));
#4149=DIRECTION('center_axis',(1.,0.,0.));
#4150=DIRECTION('ref_axis',(0.,0.,-1.));
#4151=DIRECTION('',(0.,0.,-1.));
#4152=DIRECTION('center_axis',(0.,0.,-1.));
#4153=DIRECTION('ref_axis',(-1.,0.,0.));
#4154=DIRECTION('',(0.,0.,-1.));
#4155=DIRECTION('center_axis',(0.,1.,0.));
#4156=DIRECTION('ref_axis',(0.,0.,1.));
#4157=DIRECTION('',(0.,0.,-1.));
#4158=DIRECTION('center_axis',(0.,0.,-1.));
#4159=DIRECTION('ref_axis',(-1.,0.,0.));
#4160=DIRECTION('',(0.,0.,-1.));
#4161=DIRECTION('center_axis',(-1.,0.,0.));
#4162=DIRECTION('ref_axis',(0.,0.,1.));
#4163=DIRECTION('',(0.,0.,-1.));
#4164=DIRECTION('center_axis',(0.,0.,-1.));
#4165=DIRECTION('ref_axis',(-1.,0.,0.));
#4166=DIRECTION('',(0.,0.,-1.));
#4167=DIRECTION('center_axis',(0.,1.,0.));
#4168=DIRECTION('ref_axis',(0.,0.,1.));
#4169=DIRECTION('',(0.,0.,-1.));
#4170=DIRECTION('',(1.,0.,0.));
#4171=DIRECTION('center_axis',(-1.,0.,0.));
#4172=DIRECTION('ref_axis',(0.,0.,1.));
#4173=DIRECTION('',(0.,0.,-1.));
#4174=DIRECTION('',(0.,1.,0.));
#4175=DIRECTION('center_axis',(0.,1.,0.));
#4176=DIRECTION('ref_axis',(0.,0.,1.));
#4177=DIRECTION('',(0.,0.,-1.));
#4178=DIRECTION('',(1.,0.,0.));
#4179=DIRECTION('center_axis',(0.,0.,-1.));
#4180=DIRECTION('ref_axis',(-1.,0.,0.));
#4181=DIRECTION('',(0.,0.,-1.));
#4182=DIRECTION('center_axis',(-1.,0.,0.));
#4183=DIRECTION('ref_axis',(0.,0.,1.));
#4184=DIRECTION('',(0.,0.,-1.));
#4185=DIRECTION('center_axis',(0.,0.,-1.));
#4186=DIRECTION('ref_axis',(-1.,0.,0.));
#4187=DIRECTION('',(0.,0.,-1.));
#4188=DIRECTION('center_axis',(0.,1.,0.));
#4189=DIRECTION('ref_axis',(0.,0.,1.));
#4190=DIRECTION('',(0.,0.,-1.));
#4191=DIRECTION('center_axis',(0.,0.,-1.));
#4192=DIRECTION('ref_axis',(-1.,0.,0.));
#4193=DIRECTION('',(0.,0.,-1.));
#4194=DIRECTION('center_axis',(1.,0.,0.));
#4195=DIRECTION('ref_axis',(0.,0.,-1.));
#4196=DIRECTION('',(0.,0.,-1.));
#4197=DIRECTION('center_axis',(0.,0.,-1.));
#4198=DIRECTION('ref_axis',(-1.,0.,0.));
#4199=DIRECTION('center_axis',(0.,0.,-1.));
#4200=DIRECTION('ref_axis',(-1.,0.,0.));
#4201=DIRECTION('center_axis',(0.,0.,-1.));
#4202=DIRECTION('ref_axis',(-1.,0.,0.));
#4203=DIRECTION('axis',(0.,0.,1.));
#4204=DIRECTION('refdir',(1.,0.,0.));
#4205=DIRECTION('center_axis',(1.,0.,0.));
#4206=DIRECTION('ref_axis',(0.,0.,-1.));
#4207=DIRECTION('',(0.,-1.,0.));
#4208=DIRECTION('',(0.,0.,-1.));
#4209=DIRECTION('',(0.,-1.,0.));
#4210=DIRECTION('',(0.,0.,-1.));
#4211=DIRECTION('center_axis',(0.,1.,0.));
#4212=DIRECTION('ref_axis',(0.,0.,1.));
#4213=DIRECTION('',(1.,0.,0.));
#4214=DIRECTION('',(0.,0.,-1.));
#4215=DIRECTION('',(1.,0.,0.));
#4216=DIRECTION('',(-1.,0.,1.28577838368676E-16));
#4217=DIRECTION('center_axis',(0.,1.,0.));
#4218=DIRECTION('ref_axis',(0.,0.,1.));
#4219=DIRECTION('',(1.,0.,0.));
#4220=DIRECTION('center_axis',(0.,1.,0.));
#4221=DIRECTION('ref_axis',(0.,0.,1.));
#4222=DIRECTION('',(-1.,0.,0.));
#4223=DIRECTION('center_axis',(0.,1.,0.));
#4224=DIRECTION('ref_axis',(0.,0.,1.));
#4225=DIRECTION('',(1.,0.,0.));
#4226=DIRECTION('center_axis',(0.,1.,0.));
#4227=DIRECTION('ref_axis',(0.,0.,1.));
#4228=DIRECTION('center_axis',(-1.,0.,0.));
#4229=DIRECTION('ref_axis',(0.,0.,1.));
#4230=DIRECTION('',(0.,1.,0.));
#4231=DIRECTION('',(0.,0.,-1.));
#4232=DIRECTION('',(0.,1.,0.));
#4233=DIRECTION('center_axis',(0.,-1.,0.));
#4234=DIRECTION('ref_axis',(0.,0.,-1.));
#4235=DIRECTION('',(-1.,0.,0.));
#4236=DIRECTION('',(0.,0.,-1.));
#4237=DIRECTION('',(-1.,0.,0.));
#4238=DIRECTION('center_axis',(0.,0.,-1.));
#4239=DIRECTION('ref_axis',(-1.,0.,0.));
#4240=DIRECTION('center_axis',(0.,0.,1.));
#4241=DIRECTION('ref_axis',(-1.,0.,0.));
#4242=DIRECTION('',(0.,0.,-1.));
#4243=DIRECTION('center_axis',(0.,0.,1.));
#4244=DIRECTION('ref_axis',(-1.,0.,0.));
#4245=DIRECTION('center_axis',(1.,0.,0.));
#4246=DIRECTION('ref_axis',(0.,0.,-1.));
#4247=DIRECTION('',(0.,-1.,0.));
#4248=DIRECTION('',(0.,0.,-1.));
#4249=DIRECTION('',(0.,-1.,0.));
#4250=DIRECTION('center_axis',(0.,-1.,0.));
#4251=DIRECTION('ref_axis',(0.,0.,-1.));
#4252=DIRECTION('',(-1.,0.,0.));
#4253=DIRECTION('',(0.,0.,-1.));
#4254=DIRECTION('',(-1.,0.,0.));
#4255=DIRECTION('',(1.,0.,0.));
#4256=DIRECTION('center_axis',(0.,1.,0.));
#4257=DIRECTION('ref_axis',(0.,0.,1.));
#4258=DIRECTION('',(-1.,0.,1.28577838368676E-16));
#4259=DIRECTION('center_axis',(0.,1.,0.));
#4260=DIRECTION('ref_axis',(0.,0.,1.));
#4261=DIRECTION('',(1.,0.,0.));
#4262=DIRECTION('center_axis',(0.,1.,0.));
#4263=DIRECTION('ref_axis',(0.,0.,-1.));
#4264=DIRECTION('',(-1.,0.,0.));
#4265=DIRECTION('center_axis',(0.,1.,0.));
#4266=DIRECTION('ref_axis',(0.,0.,-1.));
#4267=DIRECTION('center_axis',(0.,0.,-1.));
#4268=DIRECTION('ref_axis',(-1.,0.,0.));
#4269=DIRECTION('center_axis',(0.,0.,1.));
#4270=DIRECTION('ref_axis',(1.,0.,0.));
#4271=DIRECTION('center_axis',(0.,0.,1.));
#4272=DIRECTION('ref_axis',(1.,0.,0.));
#4273=DIRECTION('center_axis',(0.,0.,1.));
#4274=DIRECTION('ref_axis',(1.,0.,0.));
#4275=DIRECTION('center_axis',(0.,0.,1.));
#4276=DIRECTION('ref_axis',(1.,0.,0.));
#4277=DIRECTION('center_axis',(0.,1.,0.));
#4278=DIRECTION('ref_axis',(0.,0.,1.));
#4279=DIRECTION('',(0.,1.,0.));
#4280=DIRECTION('',(0.,1.,0.));
#4281=DIRECTION('center_axis',(0.,0.,-1.));
#4282=DIRECTION('ref_axis',(-1.,0.,0.));
#4283=DIRECTION('',(0.,1.,0.));
#4284=DIRECTION('center_axis',(0.,1.,0.));
#4285=DIRECTION('ref_axis',(0.,0.,1.));
#4286=DIRECTION('',(0.,1.,0.));
#4287=DIRECTION('center_axis',(0.,0.,1.));
#4288=DIRECTION('ref_axis',(1.,0.,0.));
#4289=DIRECTION('center_axis',(0.,1.,0.));
#4290=DIRECTION('ref_axis',(0.,0.,1.));
#4291=DIRECTION('',(0.,1.,0.));
#4292=DIRECTION('',(0.,1.,0.));
#4293=DIRECTION('center_axis',(-1.28577838368676E-16,0.,-1.));
#4294=DIRECTION('ref_axis',(-1.,0.,1.28577838368676E-16));
#4295=DIRECTION('',(0.,1.,0.));
#4296=DIRECTION('center_axis',(0.,1.,0.));
#4297=DIRECTION('ref_axis',(0.,0.,1.));
#4298=DIRECTION('',(0.,1.,0.));
#4299=DIRECTION('center_axis',(0.,0.,1.));
#4300=DIRECTION('ref_axis',(1.,0.,0.));
#4301=DIRECTION('axis',(0.,0.,1.));
#4302=DIRECTION('refdir',(1.,0.,0.));
#4303=DIRECTION('center_axis',(0.,0.,1.));
#4304=DIRECTION('ref_axis',(1.,0.,0.));
#4305=DIRECTION('',(0.,-1.,0.));
#4306=DIRECTION('center_axis',(0.,0.,-1.));
#4307=DIRECTION('ref_axis',(1.,0.,0.));
#4308=DIRECTION('',(-1.,-1.21734980770302E-14,0.));
#4309=DIRECTION('center_axis',(0.,0.,-1.));
#4310=DIRECTION('ref_axis',(1.,0.,0.));
#4311=DIRECTION('center_axis',(0.,0.,1.));
#4312=DIRECTION('ref_axis',(1.,0.,0.));
#4313=DIRECTION('',(1.,0.,0.));
#4314=DIRECTION('',(1.,0.,0.));
#4315=DIRECTION('',(0.,-1.,0.));
#4316=DIRECTION('center_axis',(0.,0.,-1.));
#4317=DIRECTION('ref_axis',(-1.,0.,0.));
#4318=DIRECTION('',(1.,1.21734980770302E-14,0.));
#4319=DIRECTION('center_axis',(0.,0.,-1.));
#4320=DIRECTION('ref_axis',(1.,0.,0.));
#4321=DIRECTION('',(0.,1.,0.));
#4322=DIRECTION('center_axis',(0.,0.,-1.));
#4323=DIRECTION('ref_axis',(1.,0.,0.));
#4324=DIRECTION('center_axis',(0.,0.,-1.));
#4325=DIRECTION('ref_axis',(-1.,0.,0.));
#4326=DIRECTION('',(0.,1.,0.));
#4327=DIRECTION('',(0.,1.,0.));
#4328=DIRECTION('',(-1.,0.,0.));
#4329=DIRECTION('center_axis',(0.,1.,0.));
#4330=DIRECTION('ref_axis',(0.,0.,1.));
#4331=DIRECTION('',(1.,0.,0.));
#4332=DIRECTION('',(0.,0.,-1.));
#4333=DIRECTION('',(0.,0.,-1.));
#4334=DIRECTION('',(1.,0.,0.));
#4335=DIRECTION('center_axis',(0.,1.,0.));
#4336=DIRECTION('ref_axis',(0.,0.,1.));
#4337=DIRECTION('',(-1.,0.,0.));
#4338=DIRECTION('center_axis',(0.,1.,0.));
#4339=DIRECTION('ref_axis',(0.,0.,1.));
#4340=DIRECTION('',(1.,0.,0.));
#4341=DIRECTION('center_axis',(0.,1.,0.));
#4342=DIRECTION('ref_axis',(0.,0.,1.));
#4343=DIRECTION('',(-1.,0.,5.14311353474695E-16));
#4344=DIRECTION('center_axis',(0.,1.,0.));
#4345=DIRECTION('ref_axis',(0.,0.,1.));
#4346=DIRECTION('center_axis',(1.,0.,0.));
#4347=DIRECTION('ref_axis',(0.,0.,-1.));
#4348=DIRECTION('',(0.,-1.,0.));
#4349=DIRECTION('',(0.,0.,-1.));
#4350=DIRECTION('center_axis',(0.,1.,0.));
#4351=DIRECTION('ref_axis',(0.,0.,1.));
#4352=DIRECTION('',(1.,0.,0.));
#4353=DIRECTION('',(0.,0.,-1.));
#4354=DIRECTION('center_axis',(0.,1.,0.));
#4355=DIRECTION('ref_axis',(0.,0.,1.));
#4356=DIRECTION('',(1.,0.,0.));
#4357=DIRECTION('center_axis',(0.,1.,0.));
#4358=DIRECTION('ref_axis',(0.,0.,1.));
#4359=DIRECTION('',(-1.,0.,0.));
#4360=DIRECTION('center_axis',(0.,1.,0.));
#4361=DIRECTION('ref_axis',(0.,0.,-1.));
#4362=DIRECTION('',(1.,0.,0.));
#4363=DIRECTION('center_axis',(0.,1.,0.));
#4364=DIRECTION('ref_axis',(0.,0.,-1.));
#4365=DIRECTION('',(-1.,0.,5.14311353474694E-16));
#4366=DIRECTION('center_axis',(0.,0.,-1.));
#4367=DIRECTION('ref_axis',(-1.,0.,0.));
#4368=DIRECTION('',(0.,0.,-1.));
#4369=DIRECTION('center_axis',(-1.,0.,0.));
#4370=DIRECTION('ref_axis',(0.,0.,1.));
#4371=DIRECTION('',(0.,0.,-1.));
#4372=DIRECTION('',(0.,1.,0.));
#4373=DIRECTION('center_axis',(0.,-1.,0.));
#4374=DIRECTION('ref_axis',(0.,0.,-1.));
#4375=DIRECTION('',(0.,0.,-1.));
#4376=DIRECTION('',(-1.,0.,0.));
#4377=DIRECTION('center_axis',(-1.,0.,0.));
#4378=DIRECTION('ref_axis',(0.,0.,1.));
#4379=DIRECTION('',(0.,0.,-1.));
#4380=DIRECTION('',(0.,1.,0.));
#4381=DIRECTION('center_axis',(0.,0.,-1.));
#4382=DIRECTION('ref_axis',(-1.,0.,0.));
#4383=DIRECTION('center_axis',(0.,0.,1.));
#4384=DIRECTION('ref_axis',(1.,0.,0.));
#4385=DIRECTION('center_axis',(0.,0.,1.));
#4386=DIRECTION('ref_axis',(1.,0.,0.));
#4387=DIRECTION('center_axis',(0.,1.,0.));
#4388=DIRECTION('ref_axis',(0.,0.,1.));
#4389=DIRECTION('',(0.,1.,0.));
#4390=DIRECTION('',(0.,1.,0.));
#4391=DIRECTION('center_axis',(0.,0.,1.));
#4392=DIRECTION('ref_axis',(1.,0.,0.));
#4393=DIRECTION('',(0.,1.,0.));
#4394=DIRECTION('center_axis',(0.,1.,0.));
#4395=DIRECTION('ref_axis',(0.,0.,1.));
#4396=DIRECTION('',(0.,1.,0.));
#4397=DIRECTION('center_axis',(-5.14311353474695E-16,0.,-1.));
#4398=DIRECTION('ref_axis',(-1.,0.,5.14311353474695E-16));
#4399=DIRECTION('center_axis',(0.,1.,0.));
#4400=DIRECTION('ref_axis',(0.,0.,1.));
#4401=DIRECTION('',(0.,1.,0.));
#4402=DIRECTION('',(0.,1.,0.));
#4403=DIRECTION('center_axis',(0.,0.,1.));
#4404=DIRECTION('ref_axis',(1.,0.,0.));
#4405=DIRECTION('',(0.,1.,0.));
#4406=DIRECTION('center_axis',(0.,1.,0.));
#4407=DIRECTION('ref_axis',(0.,0.,1.));
#4408=DIRECTION('',(0.,1.,0.));
#4409=DIRECTION('center_axis',(0.,0.,-1.));
#4410=DIRECTION('ref_axis',(-1.,0.,0.));
#4411=DIRECTION('axis',(0.,0.,1.));
#4412=DIRECTION('refdir',(1.,0.,0.));
#4413=DIRECTION('center_axis',(1.04083408558608E-15,1.,-2.48267427335006E-18));
#4414=DIRECTION('ref_axis',(5.16810401422229E-33,2.48267427335006E-18,1.));
#4415=DIRECTION('center_axis',(1.04083408558608E-15,1.,-2.48267427335006E-18));
#4416=DIRECTION('ref_axis',(5.16810401422229E-33,2.48267427335006E-18,1.));
#4417=DIRECTION('',(1.04083408558608E-15,1.,-2.48267427335006E-18));
#4418=DIRECTION('center_axis',(-1.04083408558608E-15,-1.,2.48267427335006E-18));
#4419=DIRECTION('ref_axis',(-2.58405200711041E-33,-2.48267427335006E-18,
-1.));
#4420=DIRECTION('center_axis',(1.04083408558608E-15,1.,-2.48267427335006E-18));
#4421=DIRECTION('ref_axis',(5.16810401422229E-33,2.48267427335006E-18,1.));
#4422=DIRECTION('center_axis',(1.04083408558608E-15,1.,-2.48267427335006E-18));
#4423=DIRECTION('ref_axis',(2.58405200711041E-33,2.48267427335006E-18,1.));
#4424=DIRECTION('',(1.04083408558608E-15,1.,-2.48267427335006E-18));
#4425=DIRECTION('center_axis',(1.04083408558608E-15,1.,-2.48267427335006E-18));
#4426=DIRECTION('ref_axis',(2.58405200711041E-33,2.48267427335006E-18,1.));
#4427=DIRECTION('center_axis',(1.44900431522769E-15,1.,-2.48267427335006E-18));
#4428=DIRECTION('ref_axis',(-1.,1.44900431522769E-15,-5.16810401422082E-33));
#4429=DIRECTION('center_axis',(1.04083408558608E-15,1.,-2.48267427335006E-18));
#4430=DIRECTION('ref_axis',(2.58405200711041E-33,2.48267427335006E-18,1.));
#4431=DIRECTION('',(1.44900431522769E-15,1.,-2.48267427335006E-18));
#4432=DIRECTION('center_axis',(1.44900431522769E-15,1.,-2.48267427335006E-18));
#4433=DIRECTION('ref_axis',(-1.,1.44900431522769E-15,-3.597405735389E-33));
#4434=DIRECTION('center_axis',(-5.64652480907605E-21,2.48267427335009E-18,
-1.));
#4435=DIRECTION('ref_axis',(-1.,-1.98254111540207E-15,5.64652480907112E-21));
#4436=DIRECTION('center_axis',(5.64652480907605E-21,-2.48267427335009E-18,
1.));
#4437=DIRECTION('ref_axis',(-1.,-1.98254111540207E-15,5.64652480907112E-21));
#4438=DIRECTION('',(-5.64652480907605E-21,2.48267427335009E-18,-1.));
#4439=DIRECTION('center_axis',(5.64652480907605E-21,-2.48267427335009E-18,
1.));
#4440=DIRECTION('ref_axis',(-1.,-1.98254111540207E-15,5.64652480907112E-21));
#4441=DIRECTION('',(-5.64652480907605E-21,2.48267427335009E-18,-1.));
#4442=DIRECTION('center_axis',(1.04083408558608E-15,1.,2.48267427335009E-18));
#4443=DIRECTION('ref_axis',(5.64652480907605E-21,-2.48267427335009E-18,
1.));
#4444=DIRECTION('',(1.,1.04083408558608E-15,5.64652480907598E-21));
#4445=DIRECTION('',(-5.64652480907605E-21,2.48267427335009E-18,-1.));
#4446=DIRECTION('',(1.,1.04083408558608E-15,5.64652480907598E-21));
#4447=DIRECTION('center_axis',(-5.64652480907605E-21,2.48267427335009E-18,
-1.));
#4448=DIRECTION('ref_axis',(-1.,-1.98254111540207E-15,5.64652480907112E-21));
#4449=DIRECTION('center_axis',(-5.64652480907605E-21,2.48267427335009E-18,
-1.));
#4450=DIRECTION('ref_axis',(1.,1.98254111540207E-15,-5.64652480907112E-21));
#4451=DIRECTION('',(-5.64652480907605E-21,2.48267427335009E-18,-1.));
#4452=DIRECTION('center_axis',(-5.64652480907605E-21,2.48267427335009E-18,
-1.));
#4453=DIRECTION('ref_axis',(1.,1.98254111540207E-15,-5.64652480907112E-21));
#4454=DIRECTION('center_axis',(1.,1.04083408558608E-15,-5.64652480907346E-21));
#4455=DIRECTION('ref_axis',(-5.64652480907605E-21,2.48267427335009E-18,
-1.));
#4456=DIRECTION('',(-1.04083408558608E-15,-1.,2.48267427335006E-18));
#4457=DIRECTION('',(-5.64652480907605E-21,2.48267427335009E-18,-1.));
#4458=DIRECTION('',(-1.04083408558608E-15,-1.,2.48267427335006E-18));
#4459=DIRECTION('center_axis',(-5.64652480907605E-21,2.48267427335009E-18,
-1.));
#4460=DIRECTION('ref_axis',(-1.,-9.91270557701033E-16,5.64652480907359E-21));
#4461=DIRECTION('center_axis',(-5.64652480907605E-21,2.48267427335009E-18,
-1.));
#4462=DIRECTION('ref_axis',(1.,9.91270557701033E-16,-5.64652480907359E-21));
#4463=DIRECTION('',(-5.64652480907605E-21,2.48267427335009E-18,-1.));
#4464=DIRECTION('center_axis',(-5.64652480907605E-21,2.48267427335009E-18,
-1.));
#4465=DIRECTION('ref_axis',(1.,9.91270557701033E-16,-5.64652480907359E-21));
#4466=DIRECTION('center_axis',(-1.04083408558608E-15,-1.,-2.48267427335009E-18));
#4467=DIRECTION('ref_axis',(-5.64652480907605E-21,2.48267427335009E-18,
-1.));
#4468=DIRECTION('',(-1.,-1.04083408558608E-15,-5.64652480907598E-21));
#4469=DIRECTION('',(-5.64652480907605E-21,2.48267427335009E-18,-1.));
#4470=DIRECTION('',(-1.,-1.04083408558608E-15,-5.64652480907598E-21));
#4471=DIRECTION('center_axis',(-5.64652480907605E-21,2.48267427335009E-18,
-1.));
#4472=DIRECTION('ref_axis',(-1.,-9.91270557701033E-16,5.64652480907359E-21));
#4473=DIRECTION('center_axis',(5.64652480907605E-21,-2.48267427335009E-18,
1.));
#4474=DIRECTION('ref_axis',(-1.,-9.91270557701033E-16,5.64652480907359E-21));
#4475=DIRECTION('',(-5.64652480907605E-21,2.48267427335009E-18,-1.));
#4476=DIRECTION('center_axis',(5.64652480907605E-21,-2.48267427335009E-18,
1.));
#4477=DIRECTION('ref_axis',(-1.,-9.91270557701033E-16,5.64652480907359E-21));
#4478=DIRECTION('center_axis',(1.,1.04083408558608E-15,-5.64652480907346E-21));
#4479=DIRECTION('ref_axis',(-5.64652480907605E-21,2.48267427335009E-18,
-1.));
#4480=DIRECTION('',(-1.04083408558608E-15,-1.,2.48267427335006E-18));
#4481=DIRECTION('',(-5.64652480907605E-21,2.48267427335009E-18,-1.));
#4482=DIRECTION('',(-1.04083408558608E-15,-1.,2.48267427335006E-18));
#4483=DIRECTION('center_axis',(-5.64652480907605E-21,2.48267427335009E-18,
-1.));
#4484=DIRECTION('ref_axis',(-1.,-9.91270557701033E-16,5.64652480907359E-21));
#4485=DIRECTION('center_axis',(5.64652480907605E-21,-2.48267427335009E-18,
1.));
#4486=DIRECTION('ref_axis',(1.,9.91270557701033E-16,-5.64652480907359E-21));
#4487=DIRECTION('',(-5.64652480907605E-21,2.48267427335009E-18,-1.));
#4488=DIRECTION('center_axis',(5.64652480907605E-21,-2.48267427335009E-18,
1.));
#4489=DIRECTION('ref_axis',(1.,9.91270557701033E-16,-5.64652480907359E-21));
#4490=DIRECTION('center_axis',(-9.84875263780381E-16,1.,-2.48267427335006E-18));
#4491=DIRECTION('ref_axis',(-1.,-9.84875263780381E-16,-5.64652480907612E-21));
#4492=DIRECTION('',(1.,9.84875263780381E-16,5.64652480907612E-21));
#4493=DIRECTION('',(-5.64652480907605E-21,2.48267427335009E-18,-1.));
#4494=DIRECTION('',(1.,9.84875263780381E-16,5.64652480907612E-21));
#4495=DIRECTION('center_axis',(-5.64652480907605E-21,2.48267427335009E-18,
-1.));
#4496=DIRECTION('ref_axis',(-1.,-9.91270557701034E-16,5.64652480907359E-21));
#4497=DIRECTION('center_axis',(5.64652480907605E-21,-2.48267427335009E-18,
1.));
#4498=DIRECTION('ref_axis',(-1.,-9.91270557701034E-16,5.64652480907359E-21));
#4499=DIRECTION('',(-5.64652480907605E-21,2.48267427335009E-18,-1.));
#4500=DIRECTION('center_axis',(5.64652480907605E-21,-2.48267427335009E-18,
1.));
#4501=DIRECTION('ref_axis',(-1.,-9.91270557701034E-16,5.64652480907359E-21));
#4502=DIRECTION('center_axis',(-1.,1.82934475648463E-15,-5.64652480908311E-21));
#4503=DIRECTION('ref_axis',(-1.82934475648463E-15,-1.,2.48267427335006E-18));
#4504=DIRECTION('',(1.82934475648463E-15,1.,-2.48267427335006E-18));
#4505=DIRECTION('',(-5.64652480907605E-21,2.48267427335009E-18,-1.));
#4506=DIRECTION('',(1.82934475648463E-15,1.,-2.48267427335006E-18));
#4507=DIRECTION('center_axis',(-5.64652480907605E-21,2.48267427335009E-18,
-1.));
#4508=DIRECTION('ref_axis',(-1.,-9.91270557701032E-16,5.64652480907359E-21));
#4509=DIRECTION('center_axis',(-5.64652480907605E-21,2.48267427335009E-18,
-1.));
#4510=DIRECTION('ref_axis',(1.,9.91270557701032E-16,-5.64652480907359E-21));
#4511=DIRECTION('',(-5.64652480907605E-21,2.48267427335009E-18,-1.));
#4512=DIRECTION('center_axis',(-5.64652480907605E-21,2.48267427335009E-18,
-1.));
#4513=DIRECTION('ref_axis',(1.,9.91270557701032E-16,-5.64652480907359E-21));
#4514=DIRECTION('center_axis',(1.04083408558608E-15,1.,2.48267427335009E-18));
#4515=DIRECTION('ref_axis',(5.64652480907605E-21,-2.48267427335009E-18,
1.));
#4516=DIRECTION('',(1.,1.04083408558608E-15,5.64652480907598E-21));
#4517=DIRECTION('',(-5.64652480907605E-21,2.48267427335009E-18,-1.));
#4518=DIRECTION('',(1.,1.04083408558608E-15,5.64652480907598E-21));
#4519=DIRECTION('center_axis',(-5.64652480907605E-21,2.48267427335009E-18,
-1.));
#4520=DIRECTION('ref_axis',(-1.,-9.91270557701032E-16,5.64652480907359E-21));
#4521=DIRECTION('center_axis',(5.64652480907605E-21,-2.48267427335009E-18,
1.));
#4522=DIRECTION('ref_axis',(-1.,-9.91270557701032E-16,5.64652480907359E-21));
#4523=DIRECTION('',(-5.64652480907605E-21,2.48267427335009E-18,-1.));
#4524=DIRECTION('center_axis',(5.64652480907605E-21,-2.48267427335009E-18,
1.));
#4525=DIRECTION('ref_axis',(-1.,-9.91270557701032E-16,5.64652480907359E-21));
#4526=DIRECTION('center_axis',(-1.,-1.04083408558608E-15,5.64652480907346E-21));
#4527=DIRECTION('ref_axis',(5.64652480907605E-21,-2.48267427335009E-18,
1.));
#4528=DIRECTION('',(1.04083408558608E-15,1.,-2.48267427335006E-18));
#4529=DIRECTION('',(-5.64652480907605E-21,2.48267427335009E-18,-1.));
#4530=DIRECTION('',(1.04083408558608E-15,1.,-2.48267427335006E-18));
#4531=DIRECTION('center_axis',(-5.64652480907605E-21,2.48267427335009E-18,
-1.));
#4532=DIRECTION('ref_axis',(-1.,-1.98254111540206E-15,5.64652480907113E-21));
#4533=DIRECTION('center_axis',(5.64652480907605E-21,-2.48267427335009E-18,
1.));
#4534=DIRECTION('ref_axis',(-1.,-1.98254111540206E-15,5.64652480907113E-21));
#4535=DIRECTION('',(-5.64652480907605E-21,2.48267427335009E-18,-1.));
#4536=DIRECTION('center_axis',(5.64652480907605E-21,-2.48267427335009E-18,
1.));
#4537=DIRECTION('ref_axis',(-1.,-1.98254111540206E-15,5.64652480907113E-21));
#4538=DIRECTION('center_axis',(6.32663855944483E-16,-1.,2.48267427335006E-18));
#4539=DIRECTION('ref_axis',(1.,6.32663855944483E-16,5.646524809077E-21));
#4540=DIRECTION('',(-1.,-6.32663855944483E-16,-5.646524809077E-21));
#4541=DIRECTION('',(-5.64652480907605E-21,2.48267427335009E-18,-1.));
#4542=DIRECTION('',(-1.,-6.32663855944483E-16,-5.646524809077E-21));
#4543=DIRECTION('center_axis',(-5.64652480907605E-21,2.48267427335009E-18,
-1.));
#4544=DIRECTION('ref_axis',(-1.,-1.98254111540206E-15,5.64652480907113E-21));
#4545=DIRECTION('center_axis',(-5.64652480907605E-21,2.48267427335009E-18,
-1.));
#4546=DIRECTION('ref_axis',(1.,1.98254111540206E-15,-5.64652480907113E-21));
#4547=DIRECTION('',(-5.64652480907605E-21,2.48267427335009E-18,-1.));
#4548=DIRECTION('center_axis',(-5.64652480907605E-21,2.48267427335009E-18,
-1.));
#4549=DIRECTION('ref_axis',(1.,1.98254111540206E-15,-5.64652480907113E-21));
#4550=DIRECTION('center_axis',(-1.,-1.04083408558608E-15,5.64652480907346E-21));
#4551=DIRECTION('ref_axis',(5.64652480907605E-21,-2.48267427335009E-18,
1.));
#4552=DIRECTION('',(1.04083408558608E-15,1.,-2.48267427335006E-18));
#4553=DIRECTION('',(-5.64652480907605E-21,2.48267427335009E-18,-1.));
#4554=DIRECTION('',(1.04083408558608E-15,1.,-2.48267427335006E-18));
#4555=DIRECTION('center_axis',(-5.64652480907605E-21,2.48267427335009E-18,
-1.));
#4556=DIRECTION('ref_axis',(-1.,-1.40184818773261E-38,5.64652480907605E-21));
#4557=DIRECTION('center_axis',(5.64652480907605E-21,-2.48267427335009E-18,
1.));
#4558=DIRECTION('ref_axis',(-1.,-2.80369637546521E-38,5.64652480907605E-21));
#4559=DIRECTION('',(-5.64652480907605E-21,2.48267427335009E-18,-1.));
#4560=DIRECTION('center_axis',(5.64652480907605E-21,-2.48267427335009E-18,
1.));
#4561=DIRECTION('ref_axis',(-1.,-1.40184818773261E-38,5.64652480907605E-21));
#4562=DIRECTION('center_axis',(-1.04083408558608E-15,-1.,-2.48267427335009E-18));
#4563=DIRECTION('ref_axis',(-5.64652480907605E-21,2.48267427335009E-18,
-1.));
#4564=DIRECTION('',(-1.,-1.04083408558608E-15,-5.64652480907598E-21));
#4565=DIRECTION('',(-5.64652480907605E-21,2.48267427335009E-18,-1.));
#4566=DIRECTION('',(-1.,-1.04083408558608E-15,-5.64652480907598E-21));
#4567=DIRECTION('center_axis',(-5.64652480907605E-21,2.48267427335009E-18,
-1.));
#4568=DIRECTION('ref_axis',(-1.,-1.40184818773261E-38,5.64652480907605E-21));
#4569=DIRECTION('center_axis',(5.64652480907605E-21,-2.48267427335009E-18,
1.));
#4570=DIRECTION('ref_axis',(-1.,-2.80369637546521E-38,5.64652480907605E-21));
#4571=DIRECTION('',(-5.64652480907605E-21,2.48267427335009E-18,-1.));
#4572=DIRECTION('center_axis',(5.64652480907605E-21,-2.48267427335009E-18,
1.));
#4573=DIRECTION('ref_axis',(-1.,-1.40184818773261E-38,5.64652480907605E-21));
#4574=DIRECTION('center_axis',(1.,1.04083408558608E-15,-5.64652480907346E-21));
#4575=DIRECTION('ref_axis',(-5.64652480907605E-21,2.48267427335009E-18,
-1.));
#4576=DIRECTION('',(-1.04083408558608E-15,-1.,2.48267427335006E-18));
#4577=DIRECTION('',(-1.04083408558608E-15,-1.,2.48267427335006E-18));
#4578=DIRECTION('center_axis',(5.6465248090734E-21,2.48267427335009E-18,
-1.));
#4579=DIRECTION('ref_axis',(-1.,-1.04083408558608E-15,-5.64652480907598E-21));
#4580=DIRECTION('center_axis',(5.6465248090734E-21,2.48267427335009E-18,
-1.));
#4581=DIRECTION('ref_axis',(-1.,-1.04083408558608E-15,-5.64652480907598E-21));
#4582=DIRECTION('axis',(0.,0.,1.));
#4583=DIRECTION('refdir',(1.,0.,0.));
#4584=DIRECTION('center_axis',(4.99667015660473E-16,1.35737578475903E-15,
-1.));
#4585=DIRECTION('ref_axis',(-1.,5.55111512312586E-17,-4.99667015660472E-16));
#4586=DIRECTION('center_axis',(-4.99667015660473E-16,-1.35737578475903E-15,
1.));
#4587=DIRECTION('ref_axis',(1.,-5.55111512312592E-17,4.99667015660473E-16));
#4588=DIRECTION('',(-4.99667015660473E-16,-1.35737578475903E-15,1.));
#4589=DIRECTION('center_axis',(-4.99667015660473E-16,-1.35737578475903E-15,
1.));
#4590=DIRECTION('ref_axis',(1.,-5.55111512312586E-17,4.99667015660473E-16));
#4591=DIRECTION('center_axis',(4.99667015660476E-16,-1.35737578475903E-15,
1.));
#4592=DIRECTION('ref_axis',(1.,-5.55111512312578E-17,-4.99667015660476E-16));
#4593=DIRECTION('center_axis',(4.99667015660476E-16,-1.35737578475903E-15,
1.));
#4594=DIRECTION('ref_axis',(1.,-5.55111512312578E-17,-4.99667015660476E-16));
#4595=DIRECTION('',(0.,0.,1.));
#4596=DIRECTION('',(1.,0.,0.));
#4597=DIRECTION('',(3.56816942561649E-20,-1.,1.17635933522453E-22));
#4598=DIRECTION('',(-2.22044604925031E-16,1.17635933522445E-22,1.));
#4599=DIRECTION('',(0.,0.,1.));
#4600=DIRECTION('',(1.,0.,0.));
#4601=DIRECTION('',(1.,0.,-3.49148133884313E-15));
#4602=DIRECTION('',(-3.49148133884313E-15,0.,-1.));
#4603=DIRECTION('',(1.,-2.08166817117217E-17,2.77555756156289E-16));
#4604=DIRECTION('',(1.97762642172553E-16,-0.648567038634043,-0.761157537174445));
#4605=DIRECTION('',(1.,0.,-3.49148133884313E-15));
#4606=DIRECTION('',(-3.49148133884313E-15,0.,-1.));
#4607=DIRECTION('',(-6.98296267768627E-15,0.,-1.));
#4608=DIRECTION('',(-1.,0.,6.98296267768627E-15));
#4609=DIRECTION('',(3.56816942561649E-20,-1.,1.17635933522453E-22));
#4610=DIRECTION('',(-2.22044604925031E-16,1.17635933522445E-22,1.));
#4611=DIRECTION('',(3.56816942561649E-20,-1.,1.17635933522453E-22));
#4612=DIRECTION('',(-2.22044604925031E-16,1.17635933522445E-22,1.));
#4613=DIRECTION('',(3.56816942561649E-20,-1.,1.17635933522453E-22));
#4614=DIRECTION('',(-2.22044604925031E-16,1.17635933522445E-22,1.));
#4615=DIRECTION('',(-6.98296267768627E-15,0.,-1.));
#4616=DIRECTION('',(-1.,0.,6.98296267768627E-15));
#4617=DIRECTION('',(3.56816942561649E-20,-1.,1.17635933522453E-22));
#4618=DIRECTION('',(-2.22044604925031E-16,1.17635933522445E-22,1.));
#4619=DIRECTION('',(3.56816942561649E-20,-1.,1.17635933522453E-22));
#4620=DIRECTION('',(-2.22044604925031E-16,1.17635933522445E-22,1.));
#4621=DIRECTION('',(3.56816942561649E-20,-1.,1.17635933522453E-22));
#4622=DIRECTION('',(-2.22044604925031E-16,1.17635933522445E-22,1.));
#4623=DIRECTION('',(3.56816942561649E-20,-1.,1.17635933522453E-22));
#4624=DIRECTION('',(-2.22044604925031E-16,1.17635933522445E-22,1.));
#4625=DIRECTION('',(1.,-2.08166817117217E-17,2.77555756156289E-16));
#4626=DIRECTION('',(1.97762642172553E-16,-0.648567038634043,-0.761157537174445));
#4627=DIRECTION('',(1.,-2.08166817117217E-17,2.77555756156289E-16));
#4628=DIRECTION('',(1.97762642172553E-16,-0.648567038634043,-0.761157537174445));
#4629=DIRECTION('',(1.,-2.08166817117217E-17,2.77555756156289E-16));
#4630=DIRECTION('',(1.97762642172553E-16,-0.648567038634043,-0.761157537174445));
#4631=DIRECTION('',(1.,-2.08166817117217E-17,2.77555756156289E-16));
#4632=DIRECTION('',(1.97762642172553E-16,-0.648567038634043,-0.761157537174445));
#4633=DIRECTION('',(1.,-2.08166817117217E-17,2.77555756156289E-16));
#4634=DIRECTION('',(1.97762642172553E-16,-0.648567038634043,-0.761157537174445));
#4635=DIRECTION('',(1.,-2.08166817117217E-17,2.77555756156289E-16));
#4636=DIRECTION('',(1.97762642172553E-16,-0.648567038634043,-0.761157537174445));
#4637=DIRECTION('',(1.,-2.08166817117217E-17,2.77555756156289E-16));
#4638=DIRECTION('',(1.97762642172553E-16,-0.648567038634043,-0.761157537174445));
#4639=CARTESIAN_POINT('',(0.,0.,0.));
#4640=CARTESIAN_POINT('',(0.,0.,0.));
#4641=CARTESIAN_POINT('Origin',(180.,0.,240.));
#4642=CARTESIAN_POINT('',(180.,0.,235.));
#4643=CARTESIAN_POINT('',(180.,0.,215.000000000027));
#4644=CARTESIAN_POINT('',(180.,0.,240.));
#4645=CARTESIAN_POINT('',(176.58,0.,235.));
#4646=CARTESIAN_POINT('',(180.,0.,235.));
#4647=CARTESIAN_POINT('',(176.58,0.,215.000000000027));
#4648=CARTESIAN_POINT('',(176.58,0.,240.));
#4649=CARTESIAN_POINT('',(180.,0.,215.000000000027));
#4650=CARTESIAN_POINT('Origin',(3.42000000000001,0.,240.));
#4651=CARTESIAN_POINT('',(3.41999999999998,0.,235.));
#4652=CARTESIAN_POINT('',(3.42000000000001,0.,215.000000000027));
#4653=CARTESIAN_POINT('',(3.42000000000001,0.,240.));
#4654=CARTESIAN_POINT('',(0.,0.,235.));
#4655=CARTESIAN_POINT('',(3.41999999999998,0.,235.));
#4656=CARTESIAN_POINT('',(0.,0.,215.000000000027));
#4657=CARTESIAN_POINT('',(0.,0.,240.));
#4658=CARTESIAN_POINT('',(3.42000000000006,0.,215.000000000027));
#4659=CARTESIAN_POINT('Origin',(4.42000000000001,76.58,2.77555756156289E-14));
#4660=CARTESIAN_POINT('',(3.42000000000001,5.,0.));
#4661=CARTESIAN_POINT('',(3.42000000000001,33.5988232943213,0.));
#4662=CARTESIAN_POINT('',(3.42000000000001,0.,0.));
#4663=CARTESIAN_POINT('',(0.,5.,0.));
#4664=CARTESIAN_POINT('',(4.42000000000001,5.,2.77555756156289E-14));
#4665=CARTESIAN_POINT('',(0.,33.5988232943213,0.));
#4666=CARTESIAN_POINT('',(0.,0.,0.));
#4667=CARTESIAN_POINT('',(3.42000000000001,33.5988232943213,0.));
#4668=CARTESIAN_POINT('Origin',(175.58,76.58,240.));
#4669=CARTESIAN_POINT('',(176.58,33.5988232943213,240.));
#4670=CARTESIAN_POINT('',(176.58,5.,240.));
#4671=CARTESIAN_POINT('',(176.58,80.,240.));
#4672=CARTESIAN_POINT('',(180.,5.,240.));
#4673=CARTESIAN_POINT('',(175.58,5.,240.));
#4674=CARTESIAN_POINT('',(180.,33.5988232943213,240.));
#4675=CARTESIAN_POINT('',(180.,80.,240.));
#4676=CARTESIAN_POINT('',(176.58,33.5988232943213,240.));
#4677=CARTESIAN_POINT('Origin',(176.58,80.,240.));
#4678=CARTESIAN_POINT('',(176.58,33.5988232943213,2.77555756156289E-14));
#4679=CARTESIAN_POINT('',(176.58,5.,2.77555756156289E-14));
#4680=CARTESIAN_POINT('',(176.58,80.,2.77555756156289E-14));
#4681=CARTESIAN_POINT('',(176.58,0.,5.00000000000003));
#4682=CARTESIAN_POINT('Origin',(176.58,5.,5.00000000000002));
#4683=CARTESIAN_POINT('',(176.58,0.,24.9999999999819));
#4684=CARTESIAN_POINT('',(176.58,0.,240.));
#4685=CARTESIAN_POINT('',(176.58,5.00000000000003,29.9999999999819));
#4686=CARTESIAN_POINT('',(176.58,0.,24.9999999999819));
#4687=CARTESIAN_POINT('',(176.58,15.8272355779969,29.9999999999819));
#4688=CARTESIAN_POINT('',(176.58,80.0000000000001,29.999999999982));
#4689=CARTESIAN_POINT('',(176.58,27.1581715176779,43.0383298828501));
#4690=CARTESIAN_POINT('',(176.58,147.413588670352,181.414348191063));
#4691=CARTESIAN_POINT('',(176.58,27.1581715176779,83.0283770568992));
#4692=CARTESIAN_POINT('',(176.58,27.1581715176779,240.));
#4693=CARTESIAN_POINT('',(176.58,32.1581715176779,88.0283770568993));
#4694=CARTESIAN_POINT('',(176.58,27.1581715176779,83.0283770568992));
#4695=CARTESIAN_POINT('',(176.58,46.064656950061,88.0283770568993));
#4696=CARTESIAN_POINT('',(176.58,80.,88.0283770568993));
#4697=CARTESIAN_POINT('',(176.58,46.064656950061,93.0283770568993));
#4698=CARTESIAN_POINT('',(176.58,46.064656950061,240.));
#4699=CARTESIAN_POINT('',(176.58,25.0874391412115,93.0283770568993));
#4700=CARTESIAN_POINT('',(176.58,80.,93.0283770568993));
#4701=CARTESIAN_POINT('',(176.58,20.0874391412115,98.0283770568993));
#4702=CARTESIAN_POINT('',(176.58,25.0874391412115,93.0283770568993));
#4703=CARTESIAN_POINT('',(176.58,20.0874391412115,139.12816035213));
#4704=CARTESIAN_POINT('',(176.58,20.0874391412115,240.));
#4705=CARTESIAN_POINT('',(176.58,25.0874391412115,144.12816035213));
#4706=CARTESIAN_POINT('',(176.58,20.0874391412115,139.12816035213));
#4707=CARTESIAN_POINT('',(176.58,46.064656950061,144.12816035213));
#4708=CARTESIAN_POINT('',(176.58,80.,144.12816035213));
#4709=CARTESIAN_POINT('',(176.58,46.064656950061,149.12816035213));
#4710=CARTESIAN_POINT('',(176.58,46.064656950061,240.));
#4711=CARTESIAN_POINT('',(176.58,32.1581715176779,149.12816035213));
#4712=CARTESIAN_POINT('',(176.58,80.,149.12816035213));
#4713=CARTESIAN_POINT('',(176.58,27.1581715176779,154.12816035213));
#4714=CARTESIAN_POINT('',(176.58,32.1581715176779,149.12816035213));
#4715=CARTESIAN_POINT('',(176.58,27.1581715176779,191.649217650476));
#4716=CARTESIAN_POINT('',(176.58,27.1581715176779,240.));
#4717=CARTESIAN_POINT('',(176.58,15.8272355779969,210.000000000027));
#4718=CARTESIAN_POINT('',(176.58,20.1295883549968,203.032213771069));
#4719=CARTESIAN_POINT('',(176.58,5.00000000000003,210.000000000027));
#4720=CARTESIAN_POINT('',(176.58,80.,210.000000000027));
#4721=CARTESIAN_POINT('',(176.58,5.00000000000003,210.000000000027));
#4722=CARTESIAN_POINT('Origin',(176.58,5.,235.));
#4723=CARTESIAN_POINT('',(176.58,37.6255077137894,237.964087142109));
#4724=CARTESIAN_POINT('Origin',(176.58,33.5988232943213,235.));
#4725=CARTESIAN_POINT('',(176.58,75.58,186.403267432539));
#4726=CARTESIAN_POINT('',(176.58,51.5453007034368,219.054179684474));
#4727=CARTESIAN_POINT('',(176.58,75.58,53.5967325674605));
#4728=CARTESIAN_POINT('',(176.58,75.58,240.));
#4729=CARTESIAN_POINT('',(176.58,37.6255077137894,2.03591285789148));
#4730=CARTESIAN_POINT('',(176.58,166.125558428947,176.602019489803));
#4731=CARTESIAN_POINT('Origin',(176.58,33.5988232943213,5.00000000000002));
#4732=CARTESIAN_POINT('Origin',(180.,0.,240.));
#4733=CARTESIAN_POINT('',(180.,0.,5.00000000000003));
#4734=CARTESIAN_POINT('',(180.,0.,5.00000000000002));
#4735=CARTESIAN_POINT('',(180.,0.,24.999999999982));
#4736=CARTESIAN_POINT('',(180.,0.,240.));
#4737=CARTESIAN_POINT('',(176.58,0.,24.9999999999819));
#4738=CARTESIAN_POINT('Origin',(180.,80.,240.));
#4739=CARTESIAN_POINT('',(180.,5.,2.77555756156289E-14));
#4740=CARTESIAN_POINT('Origin',(180.,5.,5.00000000000002));
#4741=CARTESIAN_POINT('',(180.,33.5988232943213,2.77555756156289E-14));
#4742=CARTESIAN_POINT('',(180.,80.,2.77555756156289E-14));
#4743=CARTESIAN_POINT('',(180.,37.6255077137895,2.03591285789155));
#4744=CARTESIAN_POINT('Origin',(180.,33.5988232943213,5.00000000000002));
#4745=CARTESIAN_POINT('',(180.,75.58,53.5967325674606));
#4746=CARTESIAN_POINT('',(180.,32.4824320291808,-4.95090694006743));
#4747=CARTESIAN_POINT('',(180.,75.58,186.403267432539));
#4748=CARTESIAN_POINT('',(180.,75.58,240.));
#4749=CARTESIAN_POINT('',(180.,37.6255077137894,237.964087142108));
#4750=CARTESIAN_POINT('',(180.,32.4824320291808,244.950906940067));
#4751=CARTESIAN_POINT('Origin',(180.,33.5988232943213,235.));
#4752=CARTESIAN_POINT('Origin',(180.,5.,235.));
#4753=CARTESIAN_POINT('',(180.,5.00000000000003,210.000000000027));
#4754=CARTESIAN_POINT('',(180.,27.5000000000137,187.500000000014));
#4755=CARTESIAN_POINT('',(180.,15.8272355779969,210.000000000027));
#4756=CARTESIAN_POINT('',(180.,15.8272355779969,210.000000000027));
#4757=CARTESIAN_POINT('',(180.,27.1581715176779,191.649217650476));
#4758=CARTESIAN_POINT('',(180.,27.1581715176779,191.649217650476));
#4759=CARTESIAN_POINT('',(180.,27.1581715176779,154.12816035213));
#4760=CARTESIAN_POINT('',(180.,27.1581715176779,149.12816035213));
#4761=CARTESIAN_POINT('',(180.,32.1581715176779,149.12816035213));
#4762=CARTESIAN_POINT('',(180.,10.6431659349041,170.643165934904));
#4763=CARTESIAN_POINT('',(180.,46.064656950061,149.12816035213));
#4764=CARTESIAN_POINT('',(180.,46.064656950061,149.12816035213));
#4765=CARTESIAN_POINT('',(180.,46.064656950061,144.12816035213));
#4766=CARTESIAN_POINT('',(180.,46.064656950061,144.12816035213));
#4767=CARTESIAN_POINT('',(180.,25.0874391412115,144.12816035213));
#4768=CARTESIAN_POINT('',(180.,20.0874391412115,144.12816035213));
#4769=CARTESIAN_POINT('',(180.,20.0874391412115,139.12816035213));
#4770=CARTESIAN_POINT('',(180.,100.479639394541,219.520360605459));
#4771=CARTESIAN_POINT('',(180.,20.0874391412115,98.0283770568993));
#4772=CARTESIAN_POINT('',(180.,20.0874391412115,93.0283770568993));
#4773=CARTESIAN_POINT('',(180.,25.0874391412115,93.0283770568993));
#4774=CARTESIAN_POINT('',(180.,-20.9420919009446,139.057908099055));
#4775=CARTESIAN_POINT('',(180.,46.064656950061,93.0283770568993));
#4776=CARTESIAN_POINT('',(180.,46.064656950061,93.0283770568993));
#4777=CARTESIAN_POINT('',(180.,46.064656950061,88.0283770568993));
#4778=CARTESIAN_POINT('',(180.,46.064656950061,88.0283770568993));
#4779=CARTESIAN_POINT('',(180.,32.1581715176779,88.0283770568993));
#4780=CARTESIAN_POINT('',(180.,27.1581715176779,88.0283770568993));
#4781=CARTESIAN_POINT('',(180.,27.1581715176779,83.0283770568992));
#4782=CARTESIAN_POINT('',(180.,132.064897230389,187.935102769611));
#4783=CARTESIAN_POINT('',(180.,27.1581715176779,43.0383298828501));
#4784=CARTESIAN_POINT('',(180.,27.1581715176779,43.0383298828501));
#4785=CARTESIAN_POINT('',(180.,15.8272355779969,29.999999999982));
#4786=CARTESIAN_POINT('',(180.,15.8272355779969,29.999999999982));
#4787=CARTESIAN_POINT('',(180.,5.00000000000003,29.999999999982));
#4788=CARTESIAN_POINT('',(180.,15.8272355779969,29.999999999982));
#4789=CARTESIAN_POINT('',(180.,147.500000000009,172.499999999991));
#4790=CARTESIAN_POINT('Origin',(175.58,75.58,240.));
#4791=CARTESIAN_POINT('',(175.58,80.,180.398739130653));
#4792=CARTESIAN_POINT('Origin',(175.58,75.58,186.403267432539));
#4793=CARTESIAN_POINT('',(175.58,80.,59.6012608693474));
#4794=CARTESIAN_POINT('Origin',(175.579999999999,75.5799999999997,53.5967325674601));
#4795=CARTESIAN_POINT('',(175.58,80.,240.));
#4796=CARTESIAN_POINT('Origin',(0.,80.,240.));
#4797=CARTESIAN_POINT('',(4.41999999999998,80.,180.398739130653));
#4798=CARTESIAN_POINT('',(0.,80.,180.398739130653));
#4799=CARTESIAN_POINT('',(4.41999999999998,80.,59.6012608693474));
#4800=CARTESIAN_POINT('',(-5.55111512312578E-14,80.,59.6012608693474));
#4801=CARTESIAN_POINT('',(4.42000000000001,80.,240.));
#4802=CARTESIAN_POINT('Origin',(4.42000000000001,75.58,240.));
#4803=CARTESIAN_POINT('',(-5.55111512312578E-14,75.58,186.403267432539));
#4804=CARTESIAN_POINT('Origin',(4.42000000000044,75.5799999999996,186.40326743254));
#4805=CARTESIAN_POINT('',(0.,75.58,53.5967325674605));
#4806=CARTESIAN_POINT('Origin',(4.41999999999988,75.5800000000001,53.5967325674607));
#4807=CARTESIAN_POINT('',(0.,75.58,240.));
#4808=CARTESIAN_POINT('Origin',(0.,0.,240.));
#4809=CARTESIAN_POINT('',(0.,0.,5.));
#4810=CARTESIAN_POINT('Origin',(0.,5.,5.));
#4811=CARTESIAN_POINT('',(0.,0.,24.9999999999819));
#4812=CARTESIAN_POINT('',(0.,0.,240.));
#4813=CARTESIAN_POINT('',(0.,5.00000000000003,29.9999999999819));
#4814=CARTESIAN_POINT('',(0.,107.500000000009,132.499999999991));
#4815=CARTESIAN_POINT('',(0.,15.8272355779969,29.9999999999819));
#4816=CARTESIAN_POINT('',(0.,15.8272355779969,29.9999999999819));
#4817=CARTESIAN_POINT('',(-5.55111512312578E-14,27.1581715176779,43.0383298828501));
#4818=CARTESIAN_POINT('',(0.,15.8272355779969,29.9999999999819));
#4819=CARTESIAN_POINT('',(-5.55111512312578E-14,27.1581715176779,83.0283770568992));
#4820=CARTESIAN_POINT('',(-5.55111512312578E-14,27.1581715176779,43.0383298828501));
#4821=CARTESIAN_POINT('',(0.,32.1581715176779,88.0283770568993));
#4822=CARTESIAN_POINT('',(0.,92.0648972303893,147.935102769611));
#4823=CARTESIAN_POINT('',(0.,46.064656950061,88.0283770568993));
#4824=CARTESIAN_POINT('',(0.,27.1581715176779,88.0283770568993));
#4825=CARTESIAN_POINT('',(0.,46.064656950061,93.0283770568993));
#4826=CARTESIAN_POINT('',(0.,46.064656950061,88.0283770568993));
#4827=CARTESIAN_POINT('',(0.,25.0874391412115,93.0283770568993));
#4828=CARTESIAN_POINT('',(0.,46.064656950061,93.0283770568993));
#4829=CARTESIAN_POINT('',(-5.55111512312578E-14,20.0874391412115,98.0283770568993));
#4830=CARTESIAN_POINT('',(0.,-60.9420919009446,179.057908099055));
#4831=CARTESIAN_POINT('',(0.,20.0874391412115,139.12816035213));
#4832=CARTESIAN_POINT('',(0.,20.0874391412115,93.0283770568993));
#4833=CARTESIAN_POINT('',(0.,25.0874391412115,144.12816035213));
#4834=CARTESIAN_POINT('',(0.,60.4796393945406,179.520360605459));
#4835=CARTESIAN_POINT('',(0.,46.064656950061,144.12816035213));
#4836=CARTESIAN_POINT('',(0.,20.0874391412115,144.12816035213));
#4837=CARTESIAN_POINT('',(0.,46.064656950061,149.12816035213));
#4838=CARTESIAN_POINT('',(0.,46.064656950061,144.12816035213));
#4839=CARTESIAN_POINT('',(0.,32.1581715176779,149.12816035213));
#4840=CARTESIAN_POINT('',(0.,46.064656950061,149.12816035213));
#4841=CARTESIAN_POINT('',(-5.55111512312578E-14,27.1581715176779,154.12816035213));
#4842=CARTESIAN_POINT('',(-5.55111512312578E-14,-29.3568340650959,210.643165934904));
#4843=CARTESIAN_POINT('',(0.,27.1581715176779,191.649217650476));
#4844=CARTESIAN_POINT('',(0.,27.1581715176779,149.12816035213));
#4845=CARTESIAN_POINT('',(-5.55111512312578E-14,15.8272355779969,210.000000000027));
#4846=CARTESIAN_POINT('',(0.,27.1581715176779,191.649217650476));
#4847=CARTESIAN_POINT('',(-5.55111512312578E-14,5.00000000000003,210.000000000027));
#4848=CARTESIAN_POINT('',(-5.55111512312578E-14,15.8272355779969,210.000000000027));
#4849=CARTESIAN_POINT('',(0.,-12.4999999999863,227.500000000014));
#4850=CARTESIAN_POINT('',(0.,5.,240.));
#4851=CARTESIAN_POINT('Origin',(0.,5.,235.));
#4852=CARTESIAN_POINT('',(0.,33.5988232943213,240.));
#4853=CARTESIAN_POINT('',(0.,0.,240.));
#4854=CARTESIAN_POINT('',(0.,37.6255077137894,237.964087142108));
#4855=CARTESIAN_POINT('Origin',(0.,33.5988232943213,235.));
#4856=CARTESIAN_POINT('',(0.,32.4824320291808,244.950906940067));
#4857=CARTESIAN_POINT('',(0.,37.6255077137895,2.03591285789154));
#4858=CARTESIAN_POINT('',(-5.55111512312578E-14,32.4824320291808,-4.95090694006746));
#4859=CARTESIAN_POINT('Origin',(0.,33.5988232943213,5.));
#4860=CARTESIAN_POINT('Origin',(3.42000000000001,0.,240.));
#4861=CARTESIAN_POINT('',(3.41999999999998,0.,5.));
#4862=CARTESIAN_POINT('',(3.41999999999998,0.,5.));
#4863=CARTESIAN_POINT('',(3.42000000000001,0.,24.9999999999819));
#4864=CARTESIAN_POINT('',(3.42000000000001,0.,240.));
#4865=CARTESIAN_POINT('',(0.,0.,24.9999999999819));
#4866=CARTESIAN_POINT('Origin',(3.42000000000001,0.,240.));
#4867=CARTESIAN_POINT('Origin',(3.41999999999998,5.,5.));
#4868=CARTESIAN_POINT('',(3.42000000000001,37.6255077137895,2.03591285789145));
#4869=CARTESIAN_POINT('Origin',(3.42000000000001,33.5988232943213,5.));
#4870=CARTESIAN_POINT('',(3.42000000000001,75.58,53.5967325674606));
#4871=CARTESIAN_POINT('',(3.41999999999995,138.010958153706,138.408600247967));
#4872=CARTESIAN_POINT('',(3.41999999999995,75.58,186.403267432539));
#4873=CARTESIAN_POINT('',(3.42000000000001,75.58,240.));
#4874=CARTESIAN_POINT('',(3.42000000000001,37.6255077137895,237.964087142109));
#4875=CARTESIAN_POINT('',(3.41999999999995,23.430700428196,257.247598926311));
#4876=CARTESIAN_POINT('',(3.42000000000001,33.5988232943213,240.));
#4877=CARTESIAN_POINT('Origin',(3.42000000000001,33.5988232943213,235.));
#4878=CARTESIAN_POINT('',(3.42000000000001,5.,240.));
#4879=CARTESIAN_POINT('',(3.42000000000001,0.,240.));
#4880=CARTESIAN_POINT('Origin',(3.41999999999998,5.,235.));
#4881=CARTESIAN_POINT('',(3.41999999999995,5.00000000000003,210.000000000027));
#4882=CARTESIAN_POINT('',(3.41999999999995,5.00000000000003,210.000000000027));
#4883=CARTESIAN_POINT('',(3.42000000000001,15.8272355779969,210.000000000027));
#4884=CARTESIAN_POINT('',(3.41999999999995,0.,210.000000000027));
#4885=CARTESIAN_POINT('',(3.42000000000006,27.1581715176779,191.649217650476));
#4886=CARTESIAN_POINT('',(3.42000000000001,-1.95232149327149,238.794512988463));
#4887=CARTESIAN_POINT('',(3.41999999999995,27.1581715176779,154.12816035213));
#4888=CARTESIAN_POINT('',(3.42000000000001,27.1581715176779,240.));
#4889=CARTESIAN_POINT('',(3.42000000000001,32.1581715176779,149.12816035213));
#4890=CARTESIAN_POINT('',(3.42000000000001,32.1581715176779,149.12816035213));
#4891=CARTESIAN_POINT('',(3.42000000000006,46.064656950061,149.12816035213));
#4892=CARTESIAN_POINT('',(3.42000000000001,0.,149.12816035213));
#4893=CARTESIAN_POINT('',(3.42000000000006,46.064656950061,144.12816035213));
#4894=CARTESIAN_POINT('',(3.42000000000001,46.064656950061,240.));
#4895=CARTESIAN_POINT('',(3.42000000000001,25.0874391412115,144.12816035213));
#4896=CARTESIAN_POINT('',(3.42000000000001,0.,144.12816035213));
#4897=CARTESIAN_POINT('',(3.41999999999998,20.0874391412115,139.12816035213));
#4898=CARTESIAN_POINT('',(3.41999999999998,20.0874391412115,139.12816035213));
#4899=CARTESIAN_POINT('',(3.41999999999995,20.0874391412115,98.0283770568993));
#4900=CARTESIAN_POINT('',(3.42000000000001,20.0874391412115,240.));
#4901=CARTESIAN_POINT('',(3.41999999999998,25.0874391412115,93.0283770568993));
#4902=CARTESIAN_POINT('',(3.42000000000001,25.0874391412115,93.0283770568993));
#4903=CARTESIAN_POINT('',(3.42000000000006,46.064656950061,93.0283770568993));
#4904=CARTESIAN_POINT('',(3.41999999999998,0.,93.0283770568993));
#4905=CARTESIAN_POINT('',(3.42000000000006,46.064656950061,88.0283770568993));
#4906=CARTESIAN_POINT('',(3.42000000000001,46.064656950061,240.));
#4907=CARTESIAN_POINT('',(3.42000000000001,32.1581715176779,88.0283770568993));
#4908=CARTESIAN_POINT('',(3.42000000000001,0.,88.0283770568993));
#4909=CARTESIAN_POINT('',(3.41999999999995,27.1581715176779,83.0283770568992));
#4910=CARTESIAN_POINT('',(3.41999999999995,27.1581715176779,83.0283770568992));
#4911=CARTESIAN_POINT('',(3.42000000000001,27.1581715176779,43.0383298828501));
#4912=CARTESIAN_POINT('',(3.42000000000001,27.1581715176779,240.));
#4913=CARTESIAN_POINT('',(3.42000000000006,15.8272355779969,29.9999999999819));
#4914=CARTESIAN_POINT('',(3.42000000000001,112.991281499218,141.805140389003));
#4915=CARTESIAN_POINT('',(3.42000000000001,5.00000000000003,29.9999999999819));
#4916=CARTESIAN_POINT('',(3.42000000000001,9.0205620750794E-14,29.9999999999819));
#4917=CARTESIAN_POINT('',(3.42000000000001,0.,24.9999999999819));
#4918=CARTESIAN_POINT('Origin',(4.42000000000001,75.58,240.));
#4919=CARTESIAN_POINT('',(4.42000000000001,76.58,185.044776866502));
#4920=CARTESIAN_POINT('',(4.42000000000001,76.58,54.9552231334983));
#4921=CARTESIAN_POINT('',(4.42000000000001,76.58,240.));
#4922=CARTESIAN_POINT('Origin',(4.42000000000056,75.5799999999996,186.40326743254));
#4923=CARTESIAN_POINT('Origin',(4.41999999999978,75.5800000000002,53.5967325674609));
#4924=CARTESIAN_POINT('Origin',(0.,76.58,240.));
#4925=CARTESIAN_POINT('',(175.58,76.58,185.044776866502));
#4926=CARTESIAN_POINT('',(175.58,76.58,54.9552231334984));
#4927=CARTESIAN_POINT('',(175.58,76.58,240.));
#4928=CARTESIAN_POINT('',(0.,76.58,185.044776866502));
#4929=CARTESIAN_POINT('',(0.,76.58,54.9552231334983));
#4930=CARTESIAN_POINT('Origin',(175.58,75.58,240.));
#4931=CARTESIAN_POINT('Origin',(175.580000000001,75.5800000000019,186.403267432537));
#4932=CARTESIAN_POINT('Origin',(175.58,75.5799999999998,53.5967325674603));
#4933=CARTESIAN_POINT('Origin',(175.58,75.58,240.));
#4934=CARTESIAN_POINT('',(175.58,5.,240.));
#4935=CARTESIAN_POINT('',(0.,33.5988232943213,240.));
#4936=CARTESIAN_POINT('Origin',(175.58,75.58,2.77555756156289E-14));
#4937=CARTESIAN_POINT('',(176.58,5.,2.77555756156289E-14));
#4938=CARTESIAN_POINT('',(175.58,33.5988232943213,2.77555756156289E-14));
#4939=CARTESIAN_POINT('Origin',(180.,32.4824320291808,-4.95090694006743));
#4940=CARTESIAN_POINT('',(0.,37.6255077137895,2.03591285789154));
#4941=CARTESIAN_POINT('',(180.,37.6255077137895,2.03591285789155));
#4942=CARTESIAN_POINT('Origin',(180.,32.4824320291808,244.950906940067));
#4943=CARTESIAN_POINT('',(180.,37.6255077137894,237.964087142108));
#4944=CARTESIAN_POINT('',(3.42000000000001,37.6255077137894,237.964087142109));
#4945=CARTESIAN_POINT('Origin',(180.,15.8272355779969,29.999999999982));
#4946=CARTESIAN_POINT('',(3.42000000000001,5.00000000000003,29.9999999999819));
#4947=CARTESIAN_POINT('',(180.,15.8272355779969,29.999999999982));
#4948=CARTESIAN_POINT('Origin',(180.,15.8272355779969,210.000000000027));
#4949=CARTESIAN_POINT('',(-5.55111512312578E-14,5.00000000000003,210.000000000027));
#4950=CARTESIAN_POINT('',(180.,15.8272355779969,210.000000000027));
#4951=CARTESIAN_POINT('Origin',(180.,27.1581715176779,191.649217650476));
#4952=CARTESIAN_POINT('',(180.,27.1581715176779,191.649217650476));
#4953=CARTESIAN_POINT('Origin',(180.,27.1581715176779,149.12816035213));
#4954=CARTESIAN_POINT('',(180.,27.1581715176779,154.12816035213));
#4955=CARTESIAN_POINT('Origin',(180.,46.064656950061,149.12816035213));
#4956=CARTESIAN_POINT('',(180.,32.1581715176779,149.12816035213));
#4957=CARTESIAN_POINT('',(180.,46.064656950061,149.12816035213));
#4958=CARTESIAN_POINT('Origin',(180.,46.064656950061,144.12816035213));
#4959=CARTESIAN_POINT('',(180.,46.064656950061,144.12816035213));
#4960=CARTESIAN_POINT('Origin',(180.,20.0874391412115,144.12816035213));
#4961=CARTESIAN_POINT('',(180.,25.0874391412115,144.12816035213));
#4962=CARTESIAN_POINT('Origin',(180.,20.0874391412115,93.0283770568993));
#4963=CARTESIAN_POINT('',(180.,20.0874391412115,98.0283770568993));
#4964=CARTESIAN_POINT('',(180.,20.0874391412115,139.12816035213));
#4965=CARTESIAN_POINT('Origin',(180.,46.064656950061,93.0283770568993));
#4966=CARTESIAN_POINT('',(180.,25.0874391412115,93.0283770568993));
#4967=CARTESIAN_POINT('',(180.,46.064656950061,93.0283770568993));
#4968=CARTESIAN_POINT('Origin',(180.,46.064656950061,88.0283770568993));
#4969=CARTESIAN_POINT('',(180.,46.064656950061,88.0283770568993));
#4970=CARTESIAN_POINT('Origin',(180.,27.1581715176779,88.0283770568993));
#4971=CARTESIAN_POINT('',(180.,32.1581715176779,88.0283770568993));
#4972=CARTESIAN_POINT('Origin',(180.,27.1581715176779,43.0383298828501));
#4973=CARTESIAN_POINT('',(180.,27.1581715176779,83.0283770568992));
#4974=CARTESIAN_POINT('',(180.,27.1581715176779,43.0383298828501));
#4975=CARTESIAN_POINT('Origin',(180.,15.8272355779969,29.999999999982));
#4976=CARTESIAN_POINT('Origin',(180.,15.8272355779969,29.999999999982));
#4977=CARTESIAN_POINT('',(180.,15.8272355779969,29.999999999982));
#4978=CARTESIAN_POINT('',(180.,27.1581715176779,43.0383298828501));
#4979=CARTESIAN_POINT('Origin',(180.,27.1581715176779,43.0383298828501));
#4980=CARTESIAN_POINT('',(180.,27.1581715176779,83.0283770568992));
#4981=CARTESIAN_POINT('Origin',(180.,27.1581715176779,88.0283770568993));
#4982=CARTESIAN_POINT('',(180.,32.1581715176779,88.0283770568993));
#4983=CARTESIAN_POINT('',(180.,46.064656950061,88.0283770568993));
#4984=CARTESIAN_POINT('Origin',(180.,46.064656950061,88.0283770568993));
#4985=CARTESIAN_POINT('',(180.,46.064656950061,93.0283770568993));
#4986=CARTESIAN_POINT('Origin',(180.,46.064656950061,93.0283770568993));
#4987=CARTESIAN_POINT('',(180.,25.0874391412115,93.0283770568993));
#4988=CARTESIAN_POINT('Origin',(180.,20.0874391412115,93.0283770568993));
#4989=CARTESIAN_POINT('',(180.,20.0874391412115,98.0283770568993));
#4990=CARTESIAN_POINT('',(180.,20.0874391412115,139.12816035213));
#4991=CARTESIAN_POINT('Origin',(180.,20.0874391412115,144.12816035213));
#4992=CARTESIAN_POINT('',(180.,25.0874391412115,144.12816035213));
#4993=CARTESIAN_POINT('',(180.,46.064656950061,144.12816035213));
#4994=CARTESIAN_POINT('Origin',(180.,46.064656950061,144.12816035213));
#4995=CARTESIAN_POINT('',(180.,46.064656950061,149.12816035213));
#4996=CARTESIAN_POINT('Origin',(180.,46.064656950061,149.12816035213));
#4997=CARTESIAN_POINT('',(180.,32.1581715176779,149.12816035213));
#4998=CARTESIAN_POINT('Origin',(180.,27.1581715176779,149.12816035213));
#4999=CARTESIAN_POINT('',(180.,27.1581715176779,154.12816035213));
#5000=CARTESIAN_POINT('',(180.,27.1581715176779,191.649217650476));
#5001=CARTESIAN_POINT('Origin',(180.,27.1581715176779,191.649217650476));
#5002=CARTESIAN_POINT('',(180.,15.8272355779969,210.000000000027));
#5003=CARTESIAN_POINT('Origin',(180.,15.8272355779969,210.000000000027));
#5004=CARTESIAN_POINT('',(176.58,5.00000000000003,210.000000000027));
#5005=CARTESIAN_POINT('Origin',(180.,15.8272355779969,29.999999999982));
#5006=CARTESIAN_POINT('',(180.,5.00000000000003,29.999999999982));
#5007=CARTESIAN_POINT('Origin',(180.,20.0874391412115,139.12816035213));
#5008=CARTESIAN_POINT('Origin',(180.,25.0874391412115,93.0283770568993));
#5009=CARTESIAN_POINT('Origin',(180.,27.1581715176779,83.0283770568992));
#5010=CARTESIAN_POINT('Origin',(180.,32.1581715176779,149.12816035213));
#5011=CARTESIAN_POINT('Origin',(180.,20.0874391412115,139.12816035213));
#5012=CARTESIAN_POINT('Origin',(180.,32.1581715176779,149.12816035213));
#5013=CARTESIAN_POINT('Origin',(180.,27.1581715176779,83.0283770568992));
#5014=CARTESIAN_POINT('Origin',(180.,25.0874391412115,93.0283770568993));
#5015=CARTESIAN_POINT('Origin',(180.,5.00000000000003,210.000000000027));
#5016=CARTESIAN_POINT('Origin',(3.42000000000001,0.,24.9999999999819));
#5017=CARTESIAN_POINT('Origin',(180.,0.,24.999999999982));
#5018=CARTESIAN_POINT('Origin',(180.,5.00000000000003,210.000000000027));
#5019=CARTESIAN_POINT('Origin',(4.41999999999998,5.,5.00000000000003));
#5020=CARTESIAN_POINT('Origin',(180.,33.5988232943213,5.00000000000002));
#5021=CARTESIAN_POINT('Origin',(175.58,5.,5.00000000000003));
#5022=CARTESIAN_POINT('Origin',(175.58,33.5988232943213,5.00000000000003));
#5023=CARTESIAN_POINT('Origin',(180.,5.,235.));
#5024=CARTESIAN_POINT('Origin',(180.,33.5988232943213,235.));
#5025=CARTESIAN_POINT('Origin',(3.41999999999998,5.,235.));
#5026=CARTESIAN_POINT('Origin',(180.,33.5988232943213,235.));
#5027=CARTESIAN_POINT('',(0.,0.,0.));
#5028=CARTESIAN_POINT('Origin',(25.,2.,20.));
#5029=CARTESIAN_POINT('',(25.,2.,20.));
#5030=CARTESIAN_POINT('',(28.175,2.,20.));
#5031=CARTESIAN_POINT('',(25.,2.,20.));
#5032=CARTESIAN_POINT('',(23.,0.,20.));
#5033=CARTESIAN_POINT('Origin',(23.,2.,20.));
#5034=CARTESIAN_POINT('',(23.,-3.17500000000001,20.));
#5035=CARTESIAN_POINT('',(23.,-3.17500000000001,20.));
#5036=CARTESIAN_POINT('Origin',(23.,2.,20.));
#5037=CARTESIAN_POINT('Origin',(23.,-3.17500000000001,20.));
#5038=CARTESIAN_POINT('',(25.,24.825,20.));
#5039=CARTESIAN_POINT('',(25.,0.,20.));
#5040=CARTESIAN_POINT('',(28.175,24.825,20.));
#5041=CARTESIAN_POINT('',(28.175,0.,20.));
#5042=CARTESIAN_POINT('',(28.175,24.825,20.));
#5043=CARTESIAN_POINT('Origin',(23.,0.,0.));
#5044=CARTESIAN_POINT('',(23.,0.,0.));
#5045=CARTESIAN_POINT('',(23.,-3.17500000000001,0.));
#5046=CARTESIAN_POINT('',(23.,0.,0.));
#5047=CARTESIAN_POINT('',(25.,2.,0.));
#5048=CARTESIAN_POINT('Origin',(23.,2.,0.));
#5049=CARTESIAN_POINT('',(28.175,2.,1.73472347597681E-15));
#5050=CARTESIAN_POINT('',(28.175,2.,1.73472347597681E-15));
#5051=CARTESIAN_POINT('Origin',(23.,2.,0.));
#5052=CARTESIAN_POINT('Origin',(28.175,2.,1.73472347597681E-15));
#5053=CARTESIAN_POINT('',(0.,0.,0.));
#5054=CARTESIAN_POINT('',(0.,0.,0.));
#5055=CARTESIAN_POINT('',(0.,-3.17500000000001,0.));
#5056=CARTESIAN_POINT('',(0.,-3.17500000000001,0.));
#5057=CARTESIAN_POINT('',(0.,-3.17500000000001,0.));
#5058=CARTESIAN_POINT('Origin',(30.175,30.,20.));
#5059=CARTESIAN_POINT('',(30.175,30.,20.));
#5060=CARTESIAN_POINT('',(30.175,26.825,20.));
#5061=CARTESIAN_POINT('',(30.175,30.,20.));
#5062=CARTESIAN_POINT('Origin',(30.175,24.825,20.));
#5063=CARTESIAN_POINT('Origin',(30.175,24.825,20.));
#5064=CARTESIAN_POINT('Origin',(28.175,24.825,20.));
#5065=CARTESIAN_POINT('',(93.4708296557372,30.,20.));
#5066=CARTESIAN_POINT('',(25.,30.,20.));
#5067=CARTESIAN_POINT('',(93.4708296557372,26.825,20.));
#5068=CARTESIAN_POINT('',(25.,26.825,20.));
#5069=CARTESIAN_POINT('',(93.4708296557372,26.825,20.));
#5070=CARTESIAN_POINT('Origin',(25.,24.825,0.));
#5071=CARTESIAN_POINT('',(25.,24.825,0.));
#5072=CARTESIAN_POINT('',(28.175,24.825,1.73472347597681E-15));
#5073=CARTESIAN_POINT('',(25.,24.825,0.));
#5074=CARTESIAN_POINT('',(30.175,30.,1.73472347597681E-15));
#5075=CARTESIAN_POINT('Origin',(30.175,24.825,1.73472347597681E-15));
#5076=CARTESIAN_POINT('',(30.175,26.825,1.73472347597681E-15));
#5077=CARTESIAN_POINT('',(30.175,26.825,1.73472347597681E-15));
#5078=CARTESIAN_POINT('Origin',(30.175,24.825,1.73472347597681E-15));
#5079=CARTESIAN_POINT('Origin',(30.175,26.825,1.73472347597681E-15));
#5080=CARTESIAN_POINT('',(25.,0.,0.));
#5081=CARTESIAN_POINT('',(28.175,0.,1.73472347597681E-15));
#5082=CARTESIAN_POINT('Origin',(98.6458296557372,24.825,20.));
#5083=CARTESIAN_POINT('',(98.6458296557372,24.825,20.));
#5084=CARTESIAN_POINT('',(95.4708296557372,24.825,20.));
#5085=CARTESIAN_POINT('',(98.6458296557372,24.825,20.));
#5086=CARTESIAN_POINT('Origin',(93.4708296557372,24.825,20.));
#5087=CARTESIAN_POINT('Origin',(93.4708296557372,24.825,20.));
#5088=CARTESIAN_POINT('Origin',(93.4708296557372,26.825,20.));
#5089=CARTESIAN_POINT('',(98.6458296557372,2.,20.));
#5090=CARTESIAN_POINT('',(98.6458296557372,30.,20.));
#5091=CARTESIAN_POINT('',(95.4708296557372,2.,20.));
#5092=CARTESIAN_POINT('',(95.4708296557372,30.,20.));
#5093=CARTESIAN_POINT('',(95.4708296557372,2.,20.));
#5094=CARTESIAN_POINT('Origin',(93.4708296557372,30.,1.73472347597681E-15));
#5095=CARTESIAN_POINT('',(93.4708296557372,30.,1.73472347597681E-15));
#5096=CARTESIAN_POINT('',(93.4708296557372,26.825,1.73472347597681E-15));
#5097=CARTESIAN_POINT('',(93.4708296557372,30.,1.73472347597681E-15));
#5098=CARTESIAN_POINT('',(98.6458296557372,24.825,0.));
#5099=CARTESIAN_POINT('Origin',(93.4708296557372,24.825,1.73472347597681E-15));
#5100=CARTESIAN_POINT('',(95.4708296557372,24.825,1.73472347597681E-15));
#5101=CARTESIAN_POINT('',(95.4708296557372,24.825,1.73472347597681E-15));
#5102=CARTESIAN_POINT('Origin',(93.4708296557372,24.825,1.73472347597681E-15));
#5103=CARTESIAN_POINT('Origin',(95.4708296557372,24.825,1.73472347597681E-15));
#5104=CARTESIAN_POINT('',(25.,30.,0.));
#5105=CARTESIAN_POINT('',(25.,26.825,0.));
#5106=CARTESIAN_POINT('Origin',(100.645829655737,0.,20.));
#5107=CARTESIAN_POINT('',(100.645829655737,0.,20.));
#5108=CARTESIAN_POINT('',(100.645829655737,-3.17500000000001,20.));
#5109=CARTESIAN_POINT('',(100.645829655737,0.,20.));
#5110=CARTESIAN_POINT('Origin',(100.645829655737,2.,20.));
#5111=CARTESIAN_POINT('Origin',(100.645829655737,2.,20.));
#5112=CARTESIAN_POINT('Origin',(95.4708296557372,2.,20.));
#5113=CARTESIAN_POINT('',(123.645829655737,0.,20.));
#5114=CARTESIAN_POINT('',(98.6458296557372,0.,20.));
#5115=CARTESIAN_POINT('',(123.645829655737,-3.17500000000001,20.));
#5116=CARTESIAN_POINT('',(98.6458296557372,-3.17500000000001,20.));
#5117=CARTESIAN_POINT('',(123.645829655737,0.,20.));
#5118=CARTESIAN_POINT('Origin',(98.6458296557372,2.,0.));
#5119=CARTESIAN_POINT('',(98.6458296557372,2.,0.));
#5120=CARTESIAN_POINT('',(95.4708296557372,2.,1.73472347597681E-15));
#5121=CARTESIAN_POINT('',(98.6458296557372,2.,0.));
#5122=CARTESIAN_POINT('',(100.645829655737,0.,0.));
#5123=CARTESIAN_POINT('Origin',(100.645829655737,2.,0.));
#5124=CARTESIAN_POINT('',(100.645829655737,-3.17500000000001,0.));
#5125=CARTESIAN_POINT('',(100.645829655737,-3.17500000000001,0.));
#5126=CARTESIAN_POINT('Origin',(100.645829655737,2.,0.));
#5127=CARTESIAN_POINT('Origin',(100.645829655737,-3.17500000000001,0.));
#5128=CARTESIAN_POINT('',(98.6458296557372,30.,0.));
#5129=CARTESIAN_POINT('',(95.4708296557372,30.,1.73472347597681E-15));
#5130=CARTESIAN_POINT('Origin',(98.6458296557372,-3.17500000000001,20.));
#5131=CARTESIAN_POINT('',(123.645829655737,-3.17500000000001,0.));
#5132=CARTESIAN_POINT('',(98.6458296557372,-3.17500000000001,0.));
#5133=CARTESIAN_POINT('',(123.645829655737,-3.17500000000001,20.));
#5134=CARTESIAN_POINT('',(100.645829655737,-3.17500000000001,20.));
#5135=CARTESIAN_POINT('Origin',(123.645829655737,0.,20.));
#5136=CARTESIAN_POINT('',(123.645829655737,0.,0.));
#5137=CARTESIAN_POINT('',(123.645829655737,0.,0.));
#5138=CARTESIAN_POINT('',(123.645829655737,0.,20.));
#5139=CARTESIAN_POINT('Origin',(98.6458296557372,0.,20.));
#5140=CARTESIAN_POINT('',(98.6458296557372,0.,0.));
#5141=CARTESIAN_POINT('',(100.645829655737,0.,20.));
#5142=CARTESIAN_POINT('Origin',(100.645829655737,2.,20.));
#5143=CARTESIAN_POINT('',(98.6458296557372,2.,20.));
#5144=CARTESIAN_POINT('Origin',(98.6458296557372,30.,20.));
#5145=CARTESIAN_POINT('',(98.6458296557372,24.825,20.));
#5146=CARTESIAN_POINT('Origin',(93.4708296557372,24.825,20.));
#5147=CARTESIAN_POINT('',(93.4708296557372,30.,20.));
#5148=CARTESIAN_POINT('Origin',(25.,30.,20.));
#5149=CARTESIAN_POINT('',(30.175,30.,20.));
#5150=CARTESIAN_POINT('Origin',(30.175,24.825,20.));
#5151=CARTESIAN_POINT('',(25.,24.825,20.));
#5152=CARTESIAN_POINT('Origin',(25.,0.,20.));
#5153=CARTESIAN_POINT('',(25.,2.,20.));
#5154=CARTESIAN_POINT('Origin',(23.,2.,20.));
#5155=CARTESIAN_POINT('',(23.,0.,20.));
#5156=CARTESIAN_POINT('Origin',(0.,0.,20.));
#5157=CARTESIAN_POINT('',(0.,0.,20.));
#5158=CARTESIAN_POINT('',(0.,0.,20.));
#5159=CARTESIAN_POINT('',(0.,0.,20.));
#5160=CARTESIAN_POINT('Origin',(0.,-3.17500000000001,20.));
#5161=CARTESIAN_POINT('',(0.,-3.17500000000001,20.));
#5162=CARTESIAN_POINT('',(0.,-3.17500000000001,20.));
#5163=CARTESIAN_POINT('',(0.,-3.17500000000001,20.));
#5164=CARTESIAN_POINT('Origin',(0.,-3.17500000000001,20.));
#5165=CARTESIAN_POINT('',(23.,-3.17500000000001,20.));
#5166=CARTESIAN_POINT('',(0.,-3.17500000000001,20.));
#5167=CARTESIAN_POINT('Origin',(23.,2.,20.));
#5168=CARTESIAN_POINT('',(28.175,2.,20.));
#5169=CARTESIAN_POINT('Origin',(28.175,0.,20.));
#5170=CARTESIAN_POINT('',(28.175,24.825,20.));
#5171=CARTESIAN_POINT('Origin',(30.175,24.825,20.));
#5172=CARTESIAN_POINT('',(30.175,26.825,20.));
#5173=CARTESIAN_POINT('Origin',(25.,26.825,20.));
#5174=CARTESIAN_POINT('',(93.4708296557372,26.825,20.));
#5175=CARTESIAN_POINT('Origin',(93.4708296557372,24.825,20.));
#5176=CARTESIAN_POINT('',(95.4708296557372,24.825,20.));
#5177=CARTESIAN_POINT('Origin',(95.4708296557372,30.,20.));
#5178=CARTESIAN_POINT('',(95.4708296557372,2.,20.));
#5179=CARTESIAN_POINT('Origin',(100.645829655737,2.,20.));
#5180=CARTESIAN_POINT('Origin',(100.645829655737,2.,20.));
#5181=CARTESIAN_POINT('Origin',(100.645829655737,2.,0.));
#5182=CARTESIAN_POINT('',(0.,0.,0.));
#5183=CARTESIAN_POINT('Origin',(-5.55111512312578E-14,0.,300.));
#5184=CARTESIAN_POINT('',(0.,2.49999999999998,0.));
#5185=CARTESIAN_POINT('',(0.,0.,0.));
#5186=CARTESIAN_POINT('',(0.,0.,0.));
#5187=CARTESIAN_POINT('',(-5.55111512312578E-14,0.,300.));
#5188=CARTESIAN_POINT('',(-5.55111512312578E-14,0.,300.));
#5189=CARTESIAN_POINT('',(-5.55111512312578E-14,2.49999999999998,300.));
#5190=CARTESIAN_POINT('',(-5.55111512312578E-14,0.,300.));
#5191=CARTESIAN_POINT('',(-5.55111512312578E-14,2.49999999999998,300.));
#5192=CARTESIAN_POINT('Origin',(-5.55111512312578E-14,0.,300.));
#5193=CARTESIAN_POINT('',(50.,0.,-5.55111512312578E-14));
#5194=CARTESIAN_POINT('',(0.,0.,0.));
#5195=CARTESIAN_POINT('',(50.,0.,300.));
#5196=CARTESIAN_POINT('',(50.,0.,300.));
#5197=CARTESIAN_POINT('',(-5.55111512312578E-14,0.,300.));
#5198=CARTESIAN_POINT('',(37.2416210910529,-5.55111512312578E-14,26.825));
#5199=CARTESIAN_POINT('',(10.2583789089471,-5.55111512312578E-14,26.825));
#5200=CARTESIAN_POINT('',(-2.77555756156289E-14,0.,26.825));
#5201=CARTESIAN_POINT('',(10.2583789089471,-5.55111512312578E-14,33.1749999999999));
#5202=CARTESIAN_POINT('Origin',(10.2583789089471,0.,29.9999999999999));
#5203=CARTESIAN_POINT('',(37.2416210910529,0.,33.1749999999999));
#5204=CARTESIAN_POINT('',(-5.55111512312578E-14,0.,33.1749999999999));
#5205=CARTESIAN_POINT('Origin',(37.2416210910529,0.,30.));
#5206=CARTESIAN_POINT('',(37.2416210910529,-5.55111512312578E-14,266.825));
#5207=CARTESIAN_POINT('',(10.2583789089472,-5.55111512312578E-14,266.825));
#5208=CARTESIAN_POINT('',(0.,0.,266.825));
#5209=CARTESIAN_POINT('',(10.2583789089472,-5.55111512312578E-14,273.175));
#5210=CARTESIAN_POINT('Origin',(10.2583789089472,0.,270.));
#5211=CARTESIAN_POINT('',(37.2416210910529,0.,273.175));
#5212=CARTESIAN_POINT('',(0.,0.,273.175));
#5213=CARTESIAN_POINT('Origin',(37.2416210910529,0.,270.));
#5214=CARTESIAN_POINT('Origin',(50.,0.,300.));
#5215=CARTESIAN_POINT('',(50.,30.,-5.55111512312578E-14));
#5216=CARTESIAN_POINT('',(50.,0.,-5.55111512312578E-14));
#5217=CARTESIAN_POINT('',(50.,30.,300.));
#5218=CARTESIAN_POINT('',(50.,30.,300.));
#5219=CARTESIAN_POINT('',(50.,0.,300.));
#5220=CARTESIAN_POINT('Origin',(50.,30.,300.));
#5221=CARTESIAN_POINT('',(47.5,30.,0.));
#5222=CARTESIAN_POINT('',(50.,30.,-5.55111512312578E-14));
#5223=CARTESIAN_POINT('',(47.5,30.,300.));
#5224=CARTESIAN_POINT('',(47.5,30.,300.));
#5225=CARTESIAN_POINT('',(50.,30.,300.));
#5226=CARTESIAN_POINT('Origin',(47.5,27.5,300.));
#5227=CARTESIAN_POINT('',(45.,27.5,0.));
#5228=CARTESIAN_POINT('Origin',(47.5,27.5,0.));
#5229=CARTESIAN_POINT('',(45.,27.5,300.));
#5230=CARTESIAN_POINT('',(45.,27.5,300.));
#5231=CARTESIAN_POINT('Origin',(47.5,27.5,300.));
#5232=CARTESIAN_POINT('Origin',(45.,5.,300.));
#5233=CARTESIAN_POINT('',(45.,5.,0.));
#5234=CARTESIAN_POINT('',(45.,5.,0.));
#5235=CARTESIAN_POINT('',(45.,5.,300.));
#5236=CARTESIAN_POINT('',(45.,5.,300.));
#5237=CARTESIAN_POINT('',(45.,5.,300.));
#5238=CARTESIAN_POINT('Origin',(2.49999999999997,5.,300.));
#5239=CARTESIAN_POINT('',(2.50000000000003,5.,-5.55111512312578E-14));
#5240=CARTESIAN_POINT('',(2.50000000000003,5.,-5.55111512312578E-14));
#5241=CARTESIAN_POINT('',(2.49999999999997,5.,300.));
#5242=CARTESIAN_POINT('',(2.49999999999997,5.,300.));
#5243=CARTESIAN_POINT('',(2.49999999999997,5.,300.));
#5244=CARTESIAN_POINT('',(10.2583789089471,5.,33.1749999999999));
#5245=CARTESIAN_POINT('',(37.2416210910529,5.,33.1749999999999));
#5246=CARTESIAN_POINT('',(10.2583789089471,5.,33.1749999999999));
#5247=CARTESIAN_POINT('',(10.2583789089471,5.,26.825));
#5248=CARTESIAN_POINT('Origin',(10.2583789089471,5.,29.9999999999999));
#5249=CARTESIAN_POINT('',(37.2416210910529,5.,26.825));
#5250=CARTESIAN_POINT('',(10.2583789089471,5.,26.825));
#5251=CARTESIAN_POINT('Origin',(37.2416210910529,5.,30.));
#5252=CARTESIAN_POINT('',(10.2583789089472,5.,273.175));
#5253=CARTESIAN_POINT('',(37.2416210910529,5.,273.175));
#5254=CARTESIAN_POINT('',(10.2583789089472,5.,273.175));
#5255=CARTESIAN_POINT('',(10.2583789089472,5.,266.825));
#5256=CARTESIAN_POINT('Origin',(10.2583789089472,5.,270.));
#5257=CARTESIAN_POINT('',(37.2416210910529,5.,266.825));
#5258=CARTESIAN_POINT('',(10.2583789089472,5.,266.825));
#5259=CARTESIAN_POINT('Origin',(37.2416210910529,5.,270.));
#5260=CARTESIAN_POINT('Origin',(2.49999999999995,2.5,300.));
#5261=CARTESIAN_POINT('Origin',(2.5,2.5,-5.55111512312578E-14));
#5262=CARTESIAN_POINT('Origin',(2.49999999999995,2.5,300.));
#5263=CARTESIAN_POINT('Origin',(2.49999999999995,2.5,300.));
#5264=CARTESIAN_POINT('Origin',(2.5,2.5,-5.55111512312578E-14));
#5265=CARTESIAN_POINT('Origin',(10.2583789089472,-175.,270.));
#5266=CARTESIAN_POINT('',(10.2583789089472,-175.,266.825));
#5267=CARTESIAN_POINT('',(10.2583789089472,-175.,273.175));
#5268=CARTESIAN_POINT('Origin',(10.2583789089472,-175.,266.825));
#5269=CARTESIAN_POINT('',(37.2416210910529,-175.,266.825));
#5270=CARTESIAN_POINT('Origin',(37.2416210910529,-175.,270.));
#5271=CARTESIAN_POINT('',(37.2416210910529,-175.,273.175));
#5272=CARTESIAN_POINT('Origin',(10.2583789089472,-175.,273.175));
#5273=CARTESIAN_POINT('Origin',(10.2583789089471,-175.,29.9999999999999));
#5274=CARTESIAN_POINT('',(10.2583789089471,-175.,26.825));
#5275=CARTESIAN_POINT('',(10.2583789089471,-175.,33.1749999999999));
#5276=CARTESIAN_POINT('Origin',(10.2583789089471,-175.,26.825));
#5277=CARTESIAN_POINT('',(37.2416210910529,-175.,26.825));
#5278=CARTESIAN_POINT('Origin',(37.2416210910529,-175.,30.));
#5279=CARTESIAN_POINT('',(37.2416210910529,-175.,33.1749999999999));
#5280=CARTESIAN_POINT('Origin',(10.2583789089471,-175.,33.1749999999999));
#5281=CARTESIAN_POINT('',(0.,0.,0.));
#5282=CARTESIAN_POINT('Origin',(4.42,100.,300.));
#5283=CARTESIAN_POINT('',(4.42,100.,300.));
#5284=CARTESIAN_POINT('',(4.42,96.58,300.));
#5285=CARTESIAN_POINT('',(4.42,100.,300.));
#5286=CARTESIAN_POINT('',(0.,95.5799999999999,300.));
#5287=CARTESIAN_POINT('Origin',(4.42,95.58,300.));
#5288=CARTESIAN_POINT('',(3.42,95.58,300.));
#5289=CARTESIAN_POINT('',(3.42,95.58,300.));
#5290=CARTESIAN_POINT('Origin',(4.42,95.58,300.));
#5291=CARTESIAN_POINT('Origin',(3.42,95.58,300.));
#5292=CARTESIAN_POINT('',(50.,100.,300.));
#5293=CARTESIAN_POINT('',(0.,100.,300.));
#5294=CARTESIAN_POINT('',(50.,96.58,300.));
#5295=CARTESIAN_POINT('',(0.,96.58,300.));
#5296=CARTESIAN_POINT('',(50.,100.,300.));
#5297=CARTESIAN_POINT('Origin',(0.,95.5799999999999,0.));
#5298=CARTESIAN_POINT('',(0.,95.5799999999999,0.));
#5299=CARTESIAN_POINT('',(3.42,95.58,-5.55111512312578E-14));
#5300=CARTESIAN_POINT('',(0.,95.5799999999999,0.));
#5301=CARTESIAN_POINT('',(4.42,100.,0.));
#5302=CARTESIAN_POINT('Origin',(4.42,95.58,0.));
#5303=CARTESIAN_POINT('',(4.42,96.58,0.));
#5304=CARTESIAN_POINT('',(4.42,96.58,0.));
#5305=CARTESIAN_POINT('Origin',(4.42,95.58,0.));
#5306=CARTESIAN_POINT('Origin',(4.42,96.58,0.));
#5307=CARTESIAN_POINT('',(0.,0.,0.));
#5308=CARTESIAN_POINT('',(0.,0.,0.));
#5309=CARTESIAN_POINT('',(3.42,0.,-5.55111512312578E-14));
#5310=CARTESIAN_POINT('',(3.42,0.,-5.55111512312578E-14));
#5311=CARTESIAN_POINT('',(3.42,0.,-5.55111512312578E-14));
#5312=CARTESIAN_POINT('Origin',(0.,96.58,300.));
#5313=CARTESIAN_POINT('',(50.,96.58,-5.55111512312578E-14));
#5314=CARTESIAN_POINT('',(0.,96.58,0.));
#5315=CARTESIAN_POINT('',(50.,96.58,300.));
#5316=CARTESIAN_POINT('',(4.42,96.58,300.));
#5317=CARTESIAN_POINT('',(15.4661722120008,96.58,273.175));
#5318=CARTESIAN_POINT('',(42.4494143941068,96.58,273.175));
#5319=CARTESIAN_POINT('',(0.,96.58,273.175));
#5320=CARTESIAN_POINT('',(42.4494143941069,96.58,266.825));
#5321=CARTESIAN_POINT('Origin',(42.4494143941068,96.58,270.));
#5322=CARTESIAN_POINT('',(15.4661722120007,96.58,266.825));
#5323=CARTESIAN_POINT('',(1.38777878078145E-14,96.58,266.825));
#5324=CARTESIAN_POINT('Origin',(15.4661722120008,96.58,270.));
#5325=CARTESIAN_POINT('',(15.4661722120007,96.58,33.1749999999999));
#5326=CARTESIAN_POINT('',(42.4494143941068,96.58,33.1749999999999));
#5327=CARTESIAN_POINT('',(0.,96.58,33.1749999999999));
#5328=CARTESIAN_POINT('',(42.4494143941068,96.58,26.8249999999998));
#5329=CARTESIAN_POINT('Origin',(42.4494143941068,96.58,29.9999999999998));
#5330=CARTESIAN_POINT('',(15.4661722120007,96.58,26.8249999999998));
#5331=CARTESIAN_POINT('',(-1.38777878078145E-13,96.58,26.8249999999999));
#5332=CARTESIAN_POINT('Origin',(15.4661722120007,96.58,29.9999999999999));
#5333=CARTESIAN_POINT('Origin',(50.,100.,300.));
#5334=CARTESIAN_POINT('',(50.,100.,-5.55111512312578E-14));
#5335=CARTESIAN_POINT('',(50.,100.,-5.55111512312578E-14));
#5336=CARTESIAN_POINT('',(50.,100.,300.));
#5337=CARTESIAN_POINT('Origin',(0.,100.,300.));
#5338=CARTESIAN_POINT('',(0.,100.,0.));
#5339=CARTESIAN_POINT('',(4.42,100.,300.));
#5340=CARTESIAN_POINT('',(42.4494143941068,100.,273.175));
#5341=CARTESIAN_POINT('',(42.4494143941069,100.,266.825));
#5342=CARTESIAN_POINT('Origin',(42.4494143941068,100.,270.));
#5343=CARTESIAN_POINT('',(15.4661722120008,100.,273.175));
#5344=CARTESIAN_POINT('',(42.4494143941068,100.,273.175));
#5345=CARTESIAN_POINT('',(15.4661722120007,100.,266.825));
#5346=CARTESIAN_POINT('Origin',(15.4661722120008,100.,270.));
#5347=CARTESIAN_POINT('',(42.4494143941069,100.,266.825));
#5348=CARTESIAN_POINT('',(42.4494143941068,100.,33.1749999999999));
#5349=CARTESIAN_POINT('',(42.4494143941068,100.,26.8249999999998));
#5350=CARTESIAN_POINT('Origin',(42.4494143941068,100.,29.9999999999998));
#5351=CARTESIAN_POINT('',(15.4661722120007,100.,33.1749999999999));
#5352=CARTESIAN_POINT('',(42.4494143941068,100.,33.1749999999999));
#5353=CARTESIAN_POINT('',(15.4661722120007,100.,26.8249999999999));
#5354=CARTESIAN_POINT('Origin',(15.4661722120007,100.,29.9999999999999));
#5355=CARTESIAN_POINT('',(42.4494143941068,100.,26.8249999999998));
#5356=CARTESIAN_POINT('Origin',(4.42,95.58,300.));
#5357=CARTESIAN_POINT('',(0.,95.5799999999999,300.));
#5358=CARTESIAN_POINT('Origin',(0.,0.,300.));
#5359=CARTESIAN_POINT('',(0.,0.,300.));
#5360=CARTESIAN_POINT('',(0.,0.,300.));
#5361=CARTESIAN_POINT('',(0.,0.,300.));
#5362=CARTESIAN_POINT('Origin',(3.42,0.,300.));
#5363=CARTESIAN_POINT('',(3.42,0.,300.));
#5364=CARTESIAN_POINT('',(3.42,0.,300.));
#5365=CARTESIAN_POINT('',(3.42,0.,300.));
#5366=CARTESIAN_POINT('Origin',(3.42,0.,300.));
#5367=CARTESIAN_POINT('',(3.42,95.58,300.));
#5368=CARTESIAN_POINT('',(3.42,0.,300.));
#5369=CARTESIAN_POINT('Origin',(4.42,95.58,300.));
#5370=CARTESIAN_POINT('Origin',(4.42,95.58,300.));
#5371=CARTESIAN_POINT('Origin',(4.42,95.58,0.));
#5372=CARTESIAN_POINT('Origin',(42.4494143941068,90.,29.9999999999998));
#5373=CARTESIAN_POINT('',(42.4494143941068,90.,33.1749999999999));
#5374=CARTESIAN_POINT('',(42.4494143941068,90.,26.8249999999998));
#5375=CARTESIAN_POINT('Origin',(42.4494143941068,90.,33.1749999999999));
#5376=CARTESIAN_POINT('',(15.4661722120007,90.,33.1749999999999));
#5377=CARTESIAN_POINT('Origin',(15.4661722120007,90.,29.9999999999999));
#5378=CARTESIAN_POINT('',(15.4661722120007,90.,26.8249999999999));
#5379=CARTESIAN_POINT('Origin',(42.4494143941068,90.,26.8249999999998));
#5380=CARTESIAN_POINT('Origin',(42.4494143941068,90.,270.));
#5381=CARTESIAN_POINT('',(42.4494143941068,90.,273.175));
#5382=CARTESIAN_POINT('',(42.4494143941069,90.,266.825));
#5383=CARTESIAN_POINT('Origin',(42.4494143941068,90.,273.175));
#5384=CARTESIAN_POINT('',(15.4661722120008,90.,273.175));
#5385=CARTESIAN_POINT('Origin',(15.4661722120008,90.,270.));
#5386=CARTESIAN_POINT('',(15.4661722120007,90.,266.825));
#5387=CARTESIAN_POINT('Origin',(42.4494143941069,90.,266.825));
#5388=CARTESIAN_POINT('',(0.,0.,0.));
#5389=CARTESIAN_POINT('Origin',(11.5,-1.38777878078145E-14,1.5));
#5390=CARTESIAN_POINT('',(11.5,-1.38802704820878E-14,0.50000000000001));
#5391=CARTESIAN_POINT('Origin',(11.5,-1.38777878078145E-14,1.5));
#5392=CARTESIAN_POINT('',(11.5,23.1,0.50000000000001));
#5393=CARTESIAN_POINT('',(11.5,-1.38802704820878E-14,0.50000000000001));
#5394=CARTESIAN_POINT('Origin',(11.5,23.1,1.5));
#5395=CARTESIAN_POINT('Origin',(11.5,-1.38777878078145E-14,1.5));
#5396=CARTESIAN_POINT('',(11.5,53.1,0.50000000000001));
#5397=CARTESIAN_POINT('Origin',(11.5,53.1,1.5));
#5398=CARTESIAN_POINT('',(11.5000000000001,76.2,0.50000000000001));
#5399=CARTESIAN_POINT('',(11.5,-1.38802704820878E-14,0.50000000000001));
#5400=CARTESIAN_POINT('Origin',(11.5,76.2,1.5));
#5401=CARTESIAN_POINT('Origin',(50.5,7.63278329429795E-14,1.5));
#5402=CARTESIAN_POINT('',(51.5,24.6000000000001,1.5));
#5403=CARTESIAN_POINT('Origin',(50.5,24.6000000000001,1.5));
#5404=CARTESIAN_POINT('',(51.5000000000001,51.6000000000001,1.5));
#5405=CARTESIAN_POINT('',(51.5,7.48788286277518E-14,1.5));
#5406=CARTESIAN_POINT('Origin',(50.5000000000001,51.6000000000001,1.5));
#5407=CARTESIAN_POINT('Origin',(3.5,56.6,2.99999999999995));
#5408=CARTESIAN_POINT('',(0.,56.6,0.));
#5409=CARTESIAN_POINT('',(3.50000000000003,53.1,0.));
#5410=CARTESIAN_POINT('Origin',(3.5,56.6,0.));
#5411=CARTESIAN_POINT('',(3.50000000000003,53.1,2.99999999999995));
#5412=CARTESIAN_POINT('',(3.50000000000003,53.1,2.99999999999995));
#5413=CARTESIAN_POINT('',(0.,56.6,2.99999999999995));
#5414=CARTESIAN_POINT('Origin',(3.5,56.6,2.99999999999995));
#5415=CARTESIAN_POINT('',(0.,56.6,2.99999999999995));
#5416=CARTESIAN_POINT('Origin',(21.5,53.1000000000001,2.99999999999995));
#5417=CARTESIAN_POINT('',(21.5,53.1000000000001,0.));
#5418=CARTESIAN_POINT('',(21.5,53.1000000000001,0.));
#5419=CARTESIAN_POINT('',(21.5,53.1000000000001,2.99999999999995));
#5420=CARTESIAN_POINT('',(21.5,53.1000000000001,2.99999999999995));
#5421=CARTESIAN_POINT('',(21.5,53.1000000000001,2.99999999999995));
#5422=CARTESIAN_POINT('Origin',(21.5,49.6000000000001,2.99999999999995));
#5423=CARTESIAN_POINT('',(25.,49.6,0.));
#5424=CARTESIAN_POINT('Origin',(21.5,49.6000000000001,0.));
#5425=CARTESIAN_POINT('',(25.,49.6,2.99999999999995));
#5426=CARTESIAN_POINT('',(25.,49.6,2.99999999999995));
#5427=CARTESIAN_POINT('Origin',(21.5,49.6000000000001,2.99999999999995));
#5428=CARTESIAN_POINT('Origin',(25.0000000000001,26.6000000000001,2.99999999999995));
#5429=CARTESIAN_POINT('',(25.0000000000001,26.6000000000001,0.));
#5430=CARTESIAN_POINT('',(25.0000000000001,26.6000000000001,0.));
#5431=CARTESIAN_POINT('',(25.0000000000001,26.6000000000001,2.99999999999995));
#5432=CARTESIAN_POINT('',(25.0000000000001,26.6000000000001,2.99999999999995));
#5433=CARTESIAN_POINT('',(25.0000000000001,26.6000000000001,2.99999999999995));
#5434=CARTESIAN_POINT('Origin',(21.5000000000001,26.6,2.99999999999995));
#5435=CARTESIAN_POINT('',(21.5,23.1,0.));
#5436=CARTESIAN_POINT('Origin',(21.5000000000001,26.6,0.));
#5437=CARTESIAN_POINT('',(21.5,23.1,2.99999999999995));
#5438=CARTESIAN_POINT('',(21.5,23.1,2.99999999999995));
#5439=CARTESIAN_POINT('Origin',(21.5000000000001,26.6,2.99999999999995));
#5440=CARTESIAN_POINT('Origin',(3.50000000000009,23.1,2.99999999999995));
#5441=CARTESIAN_POINT('',(3.50000000000009,23.1,0.));
#5442=CARTESIAN_POINT('',(3.50000000000009,23.1,0.));
#5443=CARTESIAN_POINT('',(3.50000000000009,23.1,2.99999999999995));
#5444=CARTESIAN_POINT('',(3.50000000000009,23.1,2.99999999999995));
#5445=CARTESIAN_POINT('',(3.50000000000009,23.1,2.99999999999995));
#5446=CARTESIAN_POINT('Origin',(3.50000000000006,19.6,2.99999999999995));
#5447=CARTESIAN_POINT('',(4.16333634234434E-14,19.6,0.));
#5448=CARTESIAN_POINT('Origin',(3.50000000000006,19.6,0.));
#5449=CARTESIAN_POINT('',(4.16333634234434E-14,19.6,2.99999999999995));
#5450=CARTESIAN_POINT('',(4.16333634234434E-14,19.6,2.99999999999995));
#5451=CARTESIAN_POINT('Origin',(3.50000000000006,19.6,2.99999999999995));
#5452=CARTESIAN_POINT('Origin',(0.,3.50000000000002,2.99999999999995));
#5453=CARTESIAN_POINT('',(0.,3.50000000000002,0.));
#5454=CARTESIAN_POINT('',(0.,3.50000000000002,0.));
#5455=CARTESIAN_POINT('',(0.,3.50000000000002,2.99999999999995));
#5456=CARTESIAN_POINT('',(0.,3.50000000000002,2.99999999999995));
#5457=CARTESIAN_POINT('',(0.,3.50000000000002,2.99999999999995));
#5458=CARTESIAN_POINT('Origin',(3.49999999999999,3.5,2.99999999999995));
#5459=CARTESIAN_POINT('',(3.50000000000002,0.,0.));
#5460=CARTESIAN_POINT('Origin',(3.49999999999999,3.5,0.));
#5461=CARTESIAN_POINT('',(3.50000000000002,0.,2.99999999999995));
#5462=CARTESIAN_POINT('',(3.50000000000002,0.,2.99999999999995));
#5463=CARTESIAN_POINT('Origin',(3.49999999999999,3.5,2.99999999999995));
#5464=CARTESIAN_POINT('Origin',(34.5,2.77555756156289E-14,2.99999999999995));
#5465=CARTESIAN_POINT('',(34.5,2.77555756156289E-14,0.));
#5466=CARTESIAN_POINT('',(34.5,2.77555756156289E-14,0.));
#5467=CARTESIAN_POINT('',(34.5,2.77555756156289E-14,2.99999999999995));
#5468=CARTESIAN_POINT('',(34.5,2.77555756156289E-14,2.99999999999995));
#5469=CARTESIAN_POINT('',(34.5,2.77555756156289E-14,2.99999999999995));
#5470=CARTESIAN_POINT('Origin',(34.5,3.50000000000003,2.99999999999995));
#5471=CARTESIAN_POINT('',(38.,3.5,0.));
#5472=CARTESIAN_POINT('Origin',(34.5,3.50000000000003,0.));
#5473=CARTESIAN_POINT('',(38.,3.5,2.99999999999995));
#5474=CARTESIAN_POINT('',(38.,3.5,2.99999999999995));
#5475=CARTESIAN_POINT('Origin',(34.5,3.50000000000003,2.99999999999995));
#5476=CARTESIAN_POINT('Origin',(38.0000000000001,21.1,2.99999999999995));
#5477=CARTESIAN_POINT('',(38.0000000000001,21.1,0.));
#5478=CARTESIAN_POINT('',(38.0000000000001,21.1,0.));
#5479=CARTESIAN_POINT('',(38.0000000000001,21.1,2.99999999999995));
#5480=CARTESIAN_POINT('',(38.0000000000001,21.1,2.99999999999995));
#5481=CARTESIAN_POINT('',(38.0000000000001,21.1,2.99999999999995));
#5482=CARTESIAN_POINT('Origin',(41.5000000000001,21.1000000000001,2.99999999999995));
#5483=CARTESIAN_POINT('',(41.5,24.6000000000001,0.));
#5484=CARTESIAN_POINT('Origin',(41.5000000000001,21.1000000000001,0.));
#5485=CARTESIAN_POINT('',(41.5,24.6000000000001,2.99999999999995));
#5486=CARTESIAN_POINT('',(41.5,24.6000000000001,2.99999999999995));
#5487=CARTESIAN_POINT('Origin',(41.5000000000001,21.1000000000001,2.99999999999995));
#5488=CARTESIAN_POINT('Origin',(58.5,24.6000000000001,2.99999999999995));
#5489=CARTESIAN_POINT('',(58.5,24.6000000000001,0.));
#5490=CARTESIAN_POINT('',(58.5,24.6000000000001,0.));
#5491=CARTESIAN_POINT('',(58.5,24.6000000000001,2.99999999999995));
#5492=CARTESIAN_POINT('',(58.5,24.6000000000001,2.99999999999995));
#5493=CARTESIAN_POINT('',(58.5,24.6000000000001,2.99999999999995));
#5494=CARTESIAN_POINT('Origin',(58.5,28.1000000000001,2.99999999999995));
#5495=CARTESIAN_POINT('',(62.,28.1000000000001,0.));
#5496=CARTESIAN_POINT('Origin',(58.5,28.1000000000001,0.));
#5497=CARTESIAN_POINT('',(62.,28.1000000000001,2.99999999999995));
#5498=CARTESIAN_POINT('',(62.,28.1000000000001,2.99999999999995));
#5499=CARTESIAN_POINT('Origin',(58.5,28.1000000000001,2.99999999999995));
#5500=CARTESIAN_POINT('Origin',(62.,48.1000000000001,2.99999999999995));
#5501=CARTESIAN_POINT('',(62.,48.1000000000001,0.));
#5502=CARTESIAN_POINT('',(62.,48.1000000000001,0.));
#5503=CARTESIAN_POINT('',(62.,48.1000000000001,2.99999999999995));
#5504=CARTESIAN_POINT('',(62.,48.1000000000001,2.99999999999995));
#5505=CARTESIAN_POINT('',(62.,48.1000000000001,2.99999999999995));
#5506=CARTESIAN_POINT('Origin',(58.5,48.1000000000001,2.99999999999995));
#5507=CARTESIAN_POINT('',(58.5,51.6000000000001,0.));
#5508=CARTESIAN_POINT('Origin',(58.5,48.1000000000001,0.));
#5509=CARTESIAN_POINT('',(58.5,51.6000000000001,2.99999999999995));
#5510=CARTESIAN_POINT('',(58.5,51.6000000000001,2.99999999999995));
#5511=CARTESIAN_POINT('Origin',(58.5,48.1000000000001,2.99999999999995));
#5512=CARTESIAN_POINT('Origin',(41.5,51.6,2.99999999999995));
#5513=CARTESIAN_POINT('',(41.5,51.6,0.));
#5514=CARTESIAN_POINT('',(41.5,51.6,0.));
#5515=CARTESIAN_POINT('',(41.5,51.6,2.99999999999995));
#5516=CARTESIAN_POINT('',(41.5,51.6,2.99999999999995));
#5517=CARTESIAN_POINT('',(41.5,51.6,2.99999999999995));
#5518=CARTESIAN_POINT('Origin',(41.5,55.1,2.99999999999995));
#5519=CARTESIAN_POINT('',(38.,55.1,0.));
#5520=CARTESIAN_POINT('Origin',(41.5,55.1,0.));
#5521=CARTESIAN_POINT('',(38.,55.1,2.99999999999995));
#5522=CARTESIAN_POINT('',(38.,55.1,2.99999999999995));
#5523=CARTESIAN_POINT('Origin',(41.5,55.1,2.99999999999995));
#5524=CARTESIAN_POINT('Origin',(38.,72.7,2.99999999999995));
#5525=CARTESIAN_POINT('',(38.,72.7,0.));
#5526=CARTESIAN_POINT('',(38.,72.7,0.));
#5527=CARTESIAN_POINT('',(38.,72.7,2.99999999999995));
#5528=CARTESIAN_POINT('',(38.,72.7,2.99999999999995));
#5529=CARTESIAN_POINT('',(38.,72.7,2.99999999999995));
#5530=CARTESIAN_POINT('Origin',(34.5,72.7000000000001,2.99999999999995));
#5531=CARTESIAN_POINT('',(34.5,76.2000000000001,0.));
#5532=CARTESIAN_POINT('Origin',(34.5,72.7000000000001,0.));
#5533=CARTESIAN_POINT('',(34.5,76.2000000000001,2.99999999999995));
#5534=CARTESIAN_POINT('',(34.5,76.2000000000001,2.99999999999995));
#5535=CARTESIAN_POINT('Origin',(34.5,72.7000000000001,2.99999999999995));
#5536=CARTESIAN_POINT('Origin',(3.50000000000009,76.2,2.99999999999995));
#5537=CARTESIAN_POINT('',(3.50000000000009,76.2,0.));
#5538=CARTESIAN_POINT('',(3.50000000000009,76.2,0.));
#5539=CARTESIAN_POINT('',(3.50000000000009,76.2,2.99999999999995));
#5540=CARTESIAN_POINT('',(3.50000000000009,76.2,2.99999999999995));
#5541=CARTESIAN_POINT('',(3.50000000000009,76.2,2.99999999999995));
#5542=CARTESIAN_POINT('Origin',(3.5000000000001,72.7,2.99999999999995));
#5543=CARTESIAN_POINT('',(4.16333634234434E-14,72.7,0.));
#5544=CARTESIAN_POINT('Origin',(3.5000000000001,72.7,0.));
#5545=CARTESIAN_POINT('',(4.16333634234434E-14,72.7,2.99999999999995));
#5546=CARTESIAN_POINT('',(4.16333634234434E-14,72.7,2.99999999999995));
#5547=CARTESIAN_POINT('Origin',(3.5000000000001,72.7,2.99999999999995));
#5548=CARTESIAN_POINT('Origin',(0.,56.6,2.99999999999995));
#5549=CARTESIAN_POINT('',(0.,56.6,0.));
#5550=CARTESIAN_POINT('',(0.,56.6,2.99999999999995));
#5551=CARTESIAN_POINT('Origin',(3.5,56.6,2.99999999999995));
#5552=CARTESIAN_POINT('Origin',(3.5,56.6,0.));
#5553=CARTESIAN_POINT('',(0.,0.,0.));
#5554=CARTESIAN_POINT('Origin',(-1.38777878078145E-14,-1.38777878078145E-14,
76.2000000000004));
#5555=CARTESIAN_POINT('',(1.00000000000002,8.93762711596783E-14,0.));
#5556=CARTESIAN_POINT('Origin',(0.,0.,0.));
#5557=CARTESIAN_POINT('',(0.999999999999986,-1.40557636389605E-14,76.2000000000004));
#5558=CARTESIAN_POINT('',(0.999999999999986,-1.40557636389605E-14,76.2000000000004));
#5559=CARTESIAN_POINT('Origin',(-1.38777878078145E-14,-1.38777878078145E-14,
76.2000000000004));
#5560=CARTESIAN_POINT('Origin',(-1.38777878078145E-14,-1.38777878078145E-14,
76.2000000000004));
#5561=CARTESIAN_POINT('Origin',(0.,0.,0.));
#5562=CARTESIAN_POINT('',(-74.782352475874,19.0250566893424,-90.));
#5563=CARTESIAN_POINT('',(40.3659015849911,18.0250566893424,-109.60331577511));
#5564=CARTESIAN_POINT('',(42.1892704672541,-81.2123646827217,-90.0637894084517));
#5565=CARTESIAN_POINT('',(-117.810729532745,2.96039973928139,193.197874360047));
#5566=CARTESIAN_POINT('',(-35.8340984150089,16.5250566893424,-98.1033157751104));
#5567=CARTESIAN_POINT('',(-6.31595266624363,86.1353997392814,168.099865438349));
#5568=CARTESIAN_POINT('',(76.3174308191633,19.0250566893424,209.999999999999));
#5569=CARTESIAN_POINT('',(40.3659015849911,18.0250566893424,-70.6033157751104));
#5570=CARTESIAN_POINT('',(40.365901584991,18.0250566893424,-31.6033157751104));
#5571=CARTESIAN_POINT('',(40.365901584991,18.0250566893424,7.39668422488958));
#5572=CARTESIAN_POINT('',(-37.8107295327444,-81.2123646827217,209.936210591549));
#5573=CARTESIAN_POINT('',(40.365901584991,18.0250566893424,46.3966842248896));
#5574=CARTESIAN_POINT('',(40.3659015849909,18.0250566893424,85.3966842248896));
#5575=CARTESIAN_POINT('',(40.3659015849909,18.0250566893424,124.39668422489));
#5576=CARTESIAN_POINT('',(40.3659015849909,18.0250566893424,163.39668422489));
#5577=CARTESIAN_POINT('',(-35.8340984150089,16.5250566893424,-59.1033157751104));
#5578=CARTESIAN_POINT('',(-35.834098415009,16.5250566893424,-20.1033157751104));
#5579=CARTESIAN_POINT('',(-35.834098415009,16.5250566893424,18.8966842248895));
#5580=CARTESIAN_POINT('',(-35.834098415009,16.5250566893424,57.8966842248896));
#5581=CARTESIAN_POINT('',(-35.834098415009,16.5250566893424,96.8966842248896));
#5582=CARTESIAN_POINT('',(-35.8340984150091,16.5250566893424,135.89668422489));
#5583=CARTESIAN_POINT('',(-35.8340984150091,16.5250566893424,174.89668422489));
#5584=UNCERTAINTY_MEASURE_WITH_UNIT(LENGTH_MEASURE(0.01),#5600,
'DISTANCE_ACCURACY_VALUE',
'Maximum model space distance between geometric entities at asserted c
onnectivities');
#5585=UNCERTAINTY_MEASURE_WITH_UNIT(LENGTH_MEASURE(0.01),#5600,
'DISTANCE_ACCURACY_VALUE',
'Maximum model space distance between geometric entities at asserted c
onnectivities');
#5586=UNCERTAINTY_MEASURE_WITH_UNIT(LENGTH_MEASURE(0.01),#5600,
'DISTANCE_ACCURACY_VALUE',
'Maximum model space distance between geometric entities at asserted c
onnectivities');
#5587=UNCERTAINTY_MEASURE_WITH_UNIT(LENGTH_MEASURE(0.01),#5600,
'DISTANCE_ACCURACY_VALUE',
'Maximum model space distance between geometric entities at asserted c
onnectivities');
#5588=UNCERTAINTY_MEASURE_WITH_UNIT(LENGTH_MEASURE(0.01),#5600,
'DISTANCE_ACCURACY_VALUE',
'Maximum model space distance between geometric entities at asserted c
onnectivities');
#5589=UNCERTAINTY_MEASURE_WITH_UNIT(LENGTH_MEASURE(0.01),#5600,
'DISTANCE_ACCURACY_VALUE',
'Maximum model space distance between geometric entities at asserted c
onnectivities');
#5590=UNCERTAINTY_MEASURE_WITH_UNIT(LENGTH_MEASURE(0.01),#5600,
'DISTANCE_ACCURACY_VALUE',
'Maximum model space distance between geometric entities at asserted c
onnectivities');
#5591=UNCERTAINTY_MEASURE_WITH_UNIT(LENGTH_MEASURE(0.01),#5600,
'DISTANCE_ACCURACY_VALUE',
'Maximum model space distance between geometric entities at asserted c
onnectivities');
#5592=(
GEOMETRIC_REPRESENTATION_CONTEXT(3)
GLOBAL_UNCERTAINTY_ASSIGNED_CONTEXT((#5584))
GLOBAL_UNIT_ASSIGNED_CONTEXT((#5600,#5602,#5603))
REPRESENTATION_CONTEXT('','3D')
);
#5593=(
GEOMETRIC_REPRESENTATION_CONTEXT(3)
GLOBAL_UNCERTAINTY_ASSIGNED_CONTEXT((#5585))
GLOBAL_UNIT_ASSIGNED_CONTEXT((#5600,#5602,#5603))
REPRESENTATION_CONTEXT('','3D')
);
#5594=(
GEOMETRIC_REPRESENTATION_CONTEXT(3)
GLOBAL_UNCERTAINTY_ASSIGNED_CONTEXT((#5586))
GLOBAL_UNIT_ASSIGNED_CONTEXT((#5600,#5602,#5603))
REPRESENTATION_CONTEXT('','3D')
);
#5595=(
GEOMETRIC_REPRESENTATION_CONTEXT(3)
GLOBAL_UNCERTAINTY_ASSIGNED_CONTEXT((#5587))
GLOBAL_UNIT_ASSIGNED_CONTEXT((#5600,#5602,#5603))
REPRESENTATION_CONTEXT('','3D')
);
#5596=(
GEOMETRIC_REPRESENTATION_CONTEXT(3)
GLOBAL_UNCERTAINTY_ASSIGNED_CONTEXT((#5588))
GLOBAL_UNIT_ASSIGNED_CONTEXT((#5600,#5602,#5603))
REPRESENTATION_CONTEXT('','3D')
);
#5597=(
GEOMETRIC_REPRESENTATION_CONTEXT(3)
GLOBAL_UNCERTAINTY_ASSIGNED_CONTEXT((#5589))
GLOBAL_UNIT_ASSIGNED_CONTEXT((#5600,#5602,#5603))
REPRESENTATION_CONTEXT('','3D')
);
#5598=(
GEOMETRIC_REPRESENTATION_CONTEXT(3)
GLOBAL_UNCERTAINTY_ASSIGNED_CONTEXT((#5590))
GLOBAL_UNIT_ASSIGNED_CONTEXT((#5600,#5602,#5603))
REPRESENTATION_CONTEXT('','3D')
);
#5599=(
GEOMETRIC_REPRESENTATION_CONTEXT(3)
GLOBAL_UNCERTAINTY_ASSIGNED_CONTEXT((#5591))
GLOBAL_UNIT_ASSIGNED_CONTEXT((#5600,#5602,#5603))
REPRESENTATION_CONTEXT('','3D')
);
#5600=(
LENGTH_UNIT()
NAMED_UNIT(*)
SI_UNIT(.MILLI.,.METRE.)
);
#5601=(
LENGTH_UNIT()
NAMED_UNIT(*)
SI_UNIT($,.METRE.)
);
#5602=(
NAMED_UNIT(*)
PLANE_ANGLE_UNIT()
SI_UNIT($,.RADIAN.)
);
#5603=(
NAMED_UNIT(*)
SI_UNIT($,.STERADIAN.)
SOLID_ANGLE_UNIT()
);
#5604=SHAPE_DEFINITION_REPRESENTATION(#5611,#5640);
#5605=SHAPE_DEFINITION_REPRESENTATION(#5612,#5641);
#5606=SHAPE_DEFINITION_REPRESENTATION(#5613,#5642);
#5607=SHAPE_DEFINITION_REPRESENTATION(#5614,#5643);
#5608=SHAPE_DEFINITION_REPRESENTATION(#5615,#5644);
#5609=SHAPE_DEFINITION_REPRESENTATION(#5616,#5645);
#5610=SHAPE_DEFINITION_REPRESENTATION(#5617,#5646);
#5611=PRODUCT_DEFINITION_SHAPE('',$,#5648);
#5612=PRODUCT_DEFINITION_SHAPE('',$,#5649);
#5613=PRODUCT_DEFINITION_SHAPE('',$,#5650);
#5614=PRODUCT_DEFINITION_SHAPE('',$,#5651);
#5615=PRODUCT_DEFINITION_SHAPE('',$,#5652);
#5616=PRODUCT_DEFINITION_SHAPE('',$,#5653);
#5617=PRODUCT_DEFINITION_SHAPE('',$,#5654);
#5618=PRODUCT_DEFINITION_SHAPE($,$,#77);
#5619=PRODUCT_DEFINITION_SHAPE($,$,#78);
#5620=PRODUCT_DEFINITION_SHAPE($,$,#79);
#5621=PRODUCT_DEFINITION_SHAPE($,$,#80);
#5622=PRODUCT_DEFINITION_SHAPE($,$,#81);
#5623=PRODUCT_DEFINITION_SHAPE($,$,#82);
#5624=PRODUCT_DEFINITION_SHAPE($,$,#83);
#5625=PRODUCT_DEFINITION_SHAPE($,$,#84);
#5626=PRODUCT_DEFINITION_SHAPE($,$,#85);
#5627=PRODUCT_DEFINITION_SHAPE($,$,#86);
#5628=PRODUCT_DEFINITION_SHAPE($,$,#87);
#5629=PRODUCT_DEFINITION_SHAPE($,$,#88);
#5630=PRODUCT_DEFINITION_SHAPE($,$,#89);
#5631=PRODUCT_DEFINITION_SHAPE($,$,#90);
#5632=PRODUCT_DEFINITION_SHAPE($,$,#91);
#5633=PRODUCT_DEFINITION_SHAPE($,$,#92);
#5634=PRODUCT_DEFINITION_SHAPE($,$,#93);
#5635=PRODUCT_DEFINITION_SHAPE($,$,#94);
#5636=PRODUCT_DEFINITION_SHAPE($,$,#95);
#5637=PRODUCT_DEFINITION_SHAPE($,$,#96);
#5638=PRODUCT_DEFINITION_SHAPE($,$,#97);
#5639=PRODUCT_DEFINITION_SHAPE($,$,#98);
#5640=SHAPE_REPRESENTATION('',(#3380,#3659,#3660,#3661,#3662,#3663,#3664,
#3665,#3666,#3667,#3668,#3669,#3670,#3671,#3672,#3673,#3674,#3675,#3676,
#3677,#3678,#3679,#3680),#5592);
#5641=SHAPE_REPRESENTATION('',(#3381),#5593);
#5642=SHAPE_REPRESENTATION('',(#3472),#5594);
#5643=SHAPE_REPRESENTATION('',(#3527),#5595);
#5644=SHAPE_REPRESENTATION('',(#3558),#5596);
#5645=SHAPE_REPRESENTATION('',(#3593),#5597);
#5646=SHAPE_REPRESENTATION('',(#3653),#5598);
#5647=PRODUCT_DEFINITION_CONTEXT('part definition',#5670,'design');
#5648=PRODUCT_DEFINITION('MAT-048','MAT-048',#5655,#5647);
#5649=PRODUCT_DEFINITION('Gauge','Gauge',#5656,#5647);
#5650=PRODUCT_DEFINITION('Handle','Handle',#5657,#5647);
#5651=PRODUCT_DEFINITION('Angle Bracket','Angle Bracket',#5658,#5647);
#5652=PRODUCT_DEFINITION('Guard','Guard',#5659,#5647);
#5653=PRODUCT_DEFINITION('Link','Link',#5660,#5647);
#5654=PRODUCT_DEFINITION('Pin','Pin',#5661,#5647);
#5655=PRODUCT_DEFINITION_FORMATION('',$,#5672);
#5656=PRODUCT_DEFINITION_FORMATION('',$,#5673);
#5657=PRODUCT_DEFINITION_FORMATION('',$,#5674);
#5658=PRODUCT_DEFINITION_FORMATION('',$,#5675);
#5659=PRODUCT_DEFINITION_FORMATION('',$,#5676);
#5660=PRODUCT_DEFINITION_FORMATION('',$,#5677);
#5661=PRODUCT_DEFINITION_FORMATION('',$,#5678);
#5662=PRODUCT_RELATED_PRODUCT_CATEGORY('MAT-048','MAT-048',(#5672));
#5663=PRODUCT_RELATED_PRODUCT_CATEGORY('Gauge','Gauge',(#5673));
#5664=PRODUCT_RELATED_PRODUCT_CATEGORY('Handle','Handle',(#5674));
#5665=PRODUCT_RELATED_PRODUCT_CATEGORY('Angle Bracket','Angle Bracket',
(#5675));
#5666=PRODUCT_RELATED_PRODUCT_CATEGORY('Guard','Guard',(#5676));
#5667=PRODUCT_RELATED_PRODUCT_CATEGORY('Link','Link',(#5677));
#5668=PRODUCT_RELATED_PRODUCT_CATEGORY('Pin','Pin',(#5678));
#5669=APPLICATION_PROTOCOL_DEFINITION('international standard',
'automotive_design',2009,#5670);
#5670=APPLICATION_CONTEXT(
'Core Data for Automotive Mechanical Design Process');
#5671=PRODUCT_CONTEXT('part definition',#5670,'mechanical');
#5672=PRODUCT('MAT-048','MAT-048','STEP AP214',(#5671));
#5673=PRODUCT('Gauge','Gauge',$,(#5671));
#5674=PRODUCT('Handle','Handle','Handle',(#5671));
#5675=PRODUCT('Angle Bracket','Angle Bracket',$,(#5671));
#5676=PRODUCT('Guard','Guard',$,(#5671));
#5677=PRODUCT('Link','Link',$,(#5671));
#5678=PRODUCT('Pin','Pin',$,(#5671));
#5679=PRESENTATION_STYLE_ASSIGNMENT((#5682));
#5680=PRESENTATION_STYLE_ASSIGNMENT((#5683));
#5681=PRESENTATION_STYLE_ASSIGNMENT((#5684));
#5682=SURFACE_STYLE_USAGE(.BOTH.,#5685);
#5683=SURFACE_STYLE_USAGE(.BOTH.,#5686);
#5684=SURFACE_STYLE_USAGE(.BOTH.,#5687);
#5685=SURFACE_SIDE_STYLE('',(#5688));
#5686=SURFACE_SIDE_STYLE('',(#5689));
#5687=SURFACE_SIDE_STYLE('',(#5690));
#5688=SURFACE_STYLE_FILL_AREA(#5691);
#5689=SURFACE_STYLE_FILL_AREA(#5692);
#5690=SURFACE_STYLE_FILL_AREA(#5693);
#5691=FILL_AREA_STYLE('Steel - Satin',(#5694));
#5692=FILL_AREA_STYLE('Opaque(97,158,199)',(#5695));
#5693=FILL_AREA_STYLE('Opaque(227,224,212)',(#5696));
#5694=FILL_AREA_STYLE_COLOUR('Steel - Satin',#5697);
#5695=FILL_AREA_STYLE_COLOUR('Opaque(97,158,199)',#5698);
#5696=FILL_AREA_STYLE_COLOUR('Opaque(227,224,212)',#5699);
#5697=COLOUR_RGB('Steel - Satin',0.627450980392157,0.627450980392157,0.627450980392157);
#5698=COLOUR_RGB('Opaque(97,158,199)',0.380392156862745,0.619607843137255,
0.780392156862745);
#5699=COLOUR_RGB('Opaque(227,224,212)',0.890196078431372,0.87843137254902,
0.831372549019608);
ENDSEC;
END-ISO-10303-21;
